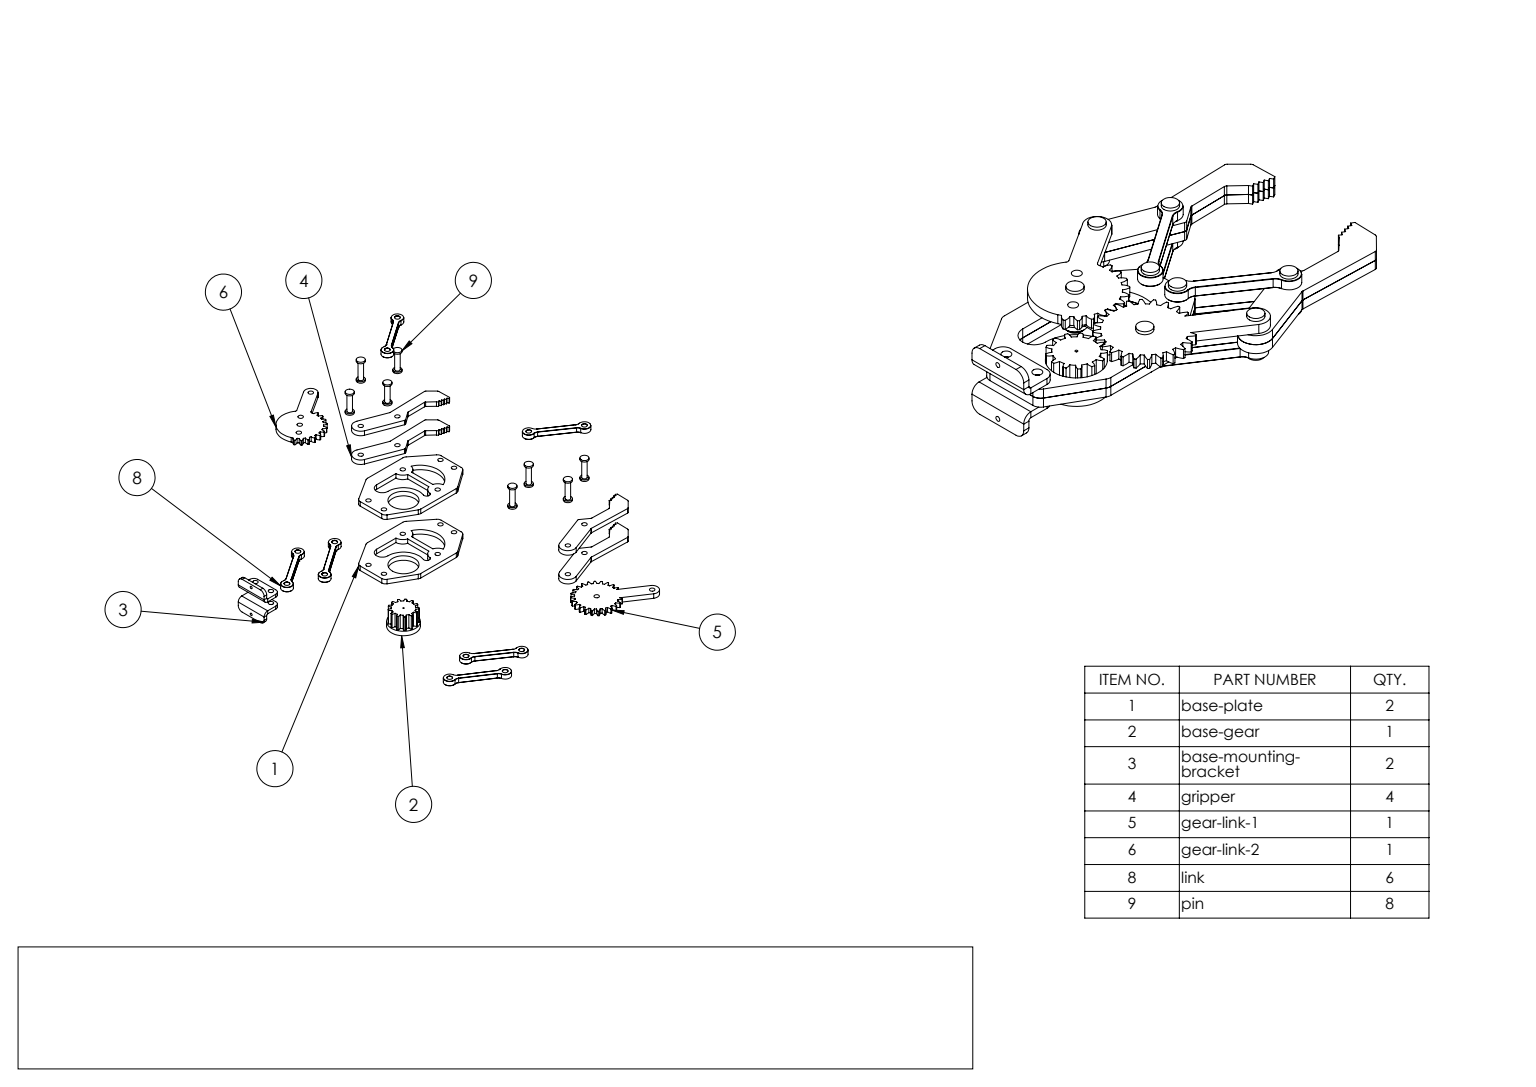
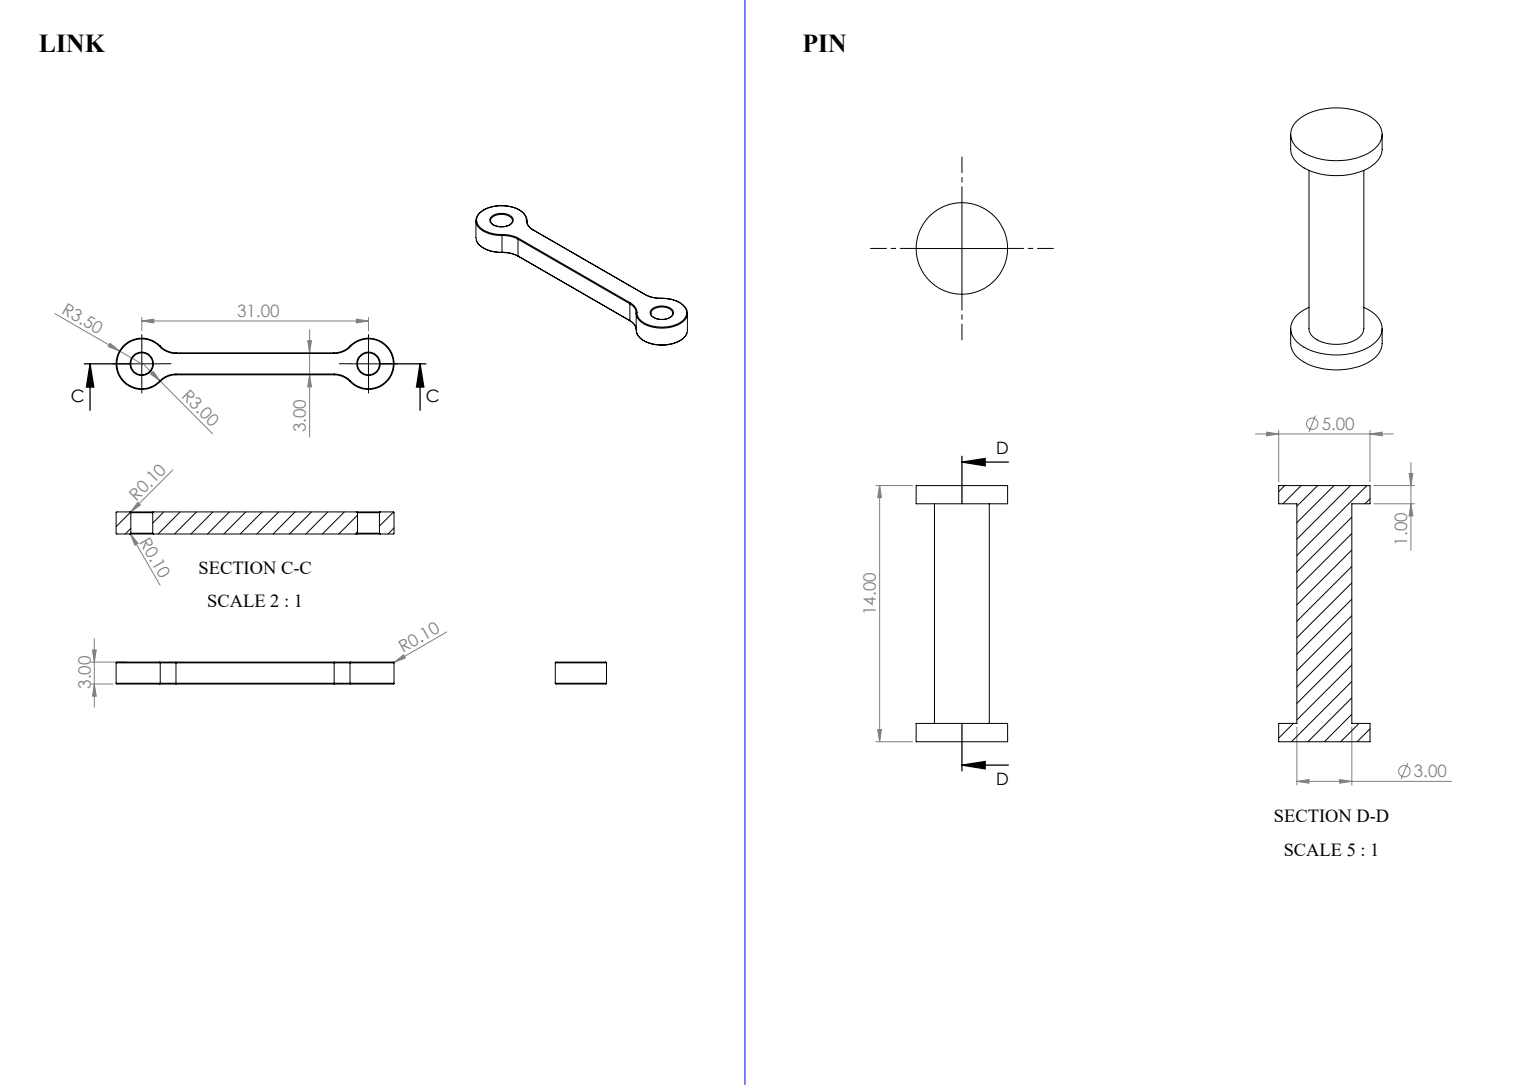
ISO-10303-21;
HEADER;
FILE_DESCRIPTION (('STEP AP214'),
    '1' );
FILE_NAME ('MAT-047',
    '2026-10-11T23:18:24',
    ( '' ),
    ( '' ),
    'SwSTEP 2.0',
    'SolidWorks 2021',
    '' );
FILE_SCHEMA (( 'AUTOMOTIVE_DESIGN' ));
ENDSEC;

DATA;
#1 = DIRECTION ( 'NONE',  ( 0.000000000000000000, 0.000000000000000000, -1.000000000000000000 ) ) ;
#2 = DIRECTION ( 'NONE',  ( 0.000000000000000000, 1.000000000000000000, 0.000000000000000000 ) ) ;
#3 = ORIENTED_EDGE ( 'NONE', *, *, #624, .T. ) ;
#4 = ORIENTED_EDGE ( 'NONE', *, *, #10369, .T. ) ;
#5 = FACE_OUTER_BOUND ( 'NONE', #2599, .T. ) ;
#6 = CIRCLE ( 'NONE', #7892, 1.600000000000000311 ) ;
#7 = EDGE_CURVE ( 'NONE', #479, #8134, #9794, .T. ) ;
#8 = ORIENTED_EDGE ( 'NONE', *, *, #949, .F. ) ;
#9 = FACE_BOUND ( 'NONE', #6807, .T. ) ;
#10 = B_SPLINE_CURVE_WITH_KNOTS ( 'NONE', 3,
 ( #6640, #5405, #12919, #3466 ),
 .UNSPECIFIED., .F., .F.,
 ( 4, 4 ),
 ( 0.1547128134717859205, 1.000000000000000000 ),
 .UNSPECIFIED. ) ;
#11 = PLANE ( 'NONE',  #4028 ) ;
#12 = DIRECTION ( 'NONE',  ( 0.000000000000000000, 0.000000000000000000, 1.000000000000000000 ) ) ;
#13 = CARTESIAN_POINT ( 'NONE',  ( 0.000000000000000000, 3.000000000000000000, 0.000000000000000000 ) ) ;
#14 = AXIS2_PLACEMENT_3D ( 'NONE', #3049, #7055, #9450 ) ;
#15 = CARTESIAN_POINT ( 'NONE',  ( 45.22938609343211880, 3.000000000000000000, -15.43472716196784233 ) ) ;
#16 = AXIS2_PLACEMENT_3D ( 'NONE', #3877, #7054, #1824 ) ;
#17 = CARTESIAN_POINT ( 'NONE',  ( 2.525608486058770641, 0.09999999999999982514, -2.423076923076923350 ) ) ;
#18 = EDGE_LOOP ( 'NONE', ( #222, #3036 ) ) ;
#19 = DIRECTION ( 'NONE',  ( -0.000000000000000000, -1.000000000000000000, -0.000000000000000000 ) ) ;
#20 = VERTEX_POINT ( 'NONE', #10251 ) ;
#21 = B_SPLINE_CURVE_WITH_KNOTS ( 'NONE', 3,
 ( #12632, #11655, #3183, #102 ),
 .UNSPECIFIED., .F., .F.,
 ( 4, 4 ),
 ( 0.1547128134717859205, 1.000000000000000000 ),
 .UNSPECIFIED. ) ;
#22 = ORIENTED_EDGE ( 'NONE', *, *, #1316, .F. ) ;
#23 = FACE_OUTER_BOUND ( 'NONE', #9551, .T. ) ;
#24 = EDGE_CURVE ( 'NONE', #4332, #3918, #6675, .T. ) ;
#25 = ORIENTED_EDGE ( 'NONE', *, *, #7176, .T. ) ;
#26 = AXIS2_PLACEMENT_3D ( 'NONE', #4384, #4937, #13276 ) ;
#27 = AXIS2_PLACEMENT_3D ( 'NONE', #4341, #12886, #6396 ) ;
#28 = DIRECTION ( 'NONE',  ( 0.000000000000000000, 1.000000000000000000, 0.000000000000000000 ) ) ;
#29 = ADVANCED_FACE ( 'NONE', ( #6308 ), #10384, .T. ) ;
#30 = DIRECTION ( 'NONE',  ( -0.000000000000000000, -1.000000000000000000, -0.000000000000000000 ) ) ;
#31 = EDGE_CURVE ( 'NONE', #5801, #5272, #8241, .T. ) ;
#32 = CARTESIAN_POINT ( 'NONE',  ( 2.458659560121117416, 9.000000000000000000, -8.136645080586040635 ) ) ;
#33 = LINE ( 'NONE', #12635, #7280 ) ;
#34 = CARTESIAN_POINT ( 'NONE',  ( 6.660877044263387781, 3.000000000000000000, -11.16999893002129696 ) ) ;
#35 = DIRECTION ( 'NONE',  ( 0.000000000000000000, 1.000000000000000000, 0.000000000000000000 ) ) ;
#36 = CARTESIAN_POINT ( 'NONE',  ( -3.835481108877868195, 0.000000000000000000, 5.554420281491219136 ) ) ;
#37 = FACE_OUTER_BOUND ( 'NONE', #7927, .T. ) ;
#38 = ORIENTED_EDGE ( 'NONE', *, *, #5654, .F. ) ;
#39 = CYLINDRICAL_SURFACE ( 'NONE', #3345, 6.750000000000000888 ) ;
#40 = AXIS2_PLACEMENT_3D ( 'NONE', #1430, #2390, #10728 ) ;
#41 = VECTOR ( 'NONE', #1784, 1000.000000000000000 ) ;
#42 = EDGE_LOOP ( 'NONE', ( #11575, #10640, #9047, #10732 ) ) ;
#43 = VERTEX_POINT ( 'NONE', #6242 ) ;
#44 = EDGE_CURVE ( 'NONE', #672, #1296, #10164, .T. ) ;
#45 = VERTEX_POINT ( 'NONE', #5075 ) ;
#46 = EDGE_LOOP ( 'NONE', ( #628, #4486, #10003, #7666 ) ) ;
#47 = FACE_BOUND ( 'NONE', #7549, .T. ) ;
#48 = DIRECTION ( 'NONE',  ( 0.000000000000000000, 1.000000000000000000, 0.000000000000000000 ) ) ;
#49 = EDGE_CURVE ( 'NONE', #1339, #3948, #9205, .T. ) ;
#50 = CIRCLE ( 'NONE', #7727, 3.000000000000000000 ) ;
#51 = FACE_OUTER_BOUND ( 'NONE', #63, .T. ) ;
#52 = B_SPLINE_CURVE_WITH_KNOTS ( 'NONE', 3,
 ( #4525, #5550, #8714, #7882 ),
 .UNSPECIFIED., .F., .F.,
 ( 4, 4 ),
 ( 0.6363612417694253232, 0.6657793188270956231 ),
 .UNSPECIFIED. ) ;
#53 = CARTESIAN_POINT ( 'NONE',  ( 0.000000000000000000, 3.000000000000000000, 0.000000000000000000 ) ) ;
#54 = CARTESIAN_POINT ( 'NONE',  ( 41.29994854050690378, 3.000000000000000000, -5.141175130212632283 ) ) ;
#55 = CARTESIAN_POINT ( 'NONE',  ( -4.564691384634503635, 3.000000000000000000, 12.76342233970727769 ) ) ;
#56 = EDGE_LOOP ( 'NONE', ( #12824, #10379, #9147, #863 ) ) ;
#57 = ORIENTED_EDGE ( 'NONE', *, *, #11037, .F. ) ;
#58 = VECTOR ( 'NONE', #8688, 1000.000000000000000 ) ;
#59 = ADVANCED_FACE ( 'NONE', ( #12400 ), #9143, .T. ) ;
#60 = DIRECTION ( 'NONE',  ( -0.000000000000000000, -1.000000000000000000, -0.000000000000000000 ) ) ;
#61 = EDGE_CURVE ( 'NONE', #8421, #357, #9412, .T. ) ;
#62 = B_SPLINE_SURFACE_WITH_KNOTS ( 'NONE', 3, 1, ( 
 ( #3640, #12274 ),
 ( #3773, #7979 ),
 ( #12201, #7023 ),
 ( #11219, #1791 ) ),
 .UNSPECIFIED., .F., .F., .F.,
 ( 4, 4 ),
 ( 2, 2 ),
 ( 0.1276832474596304168, 1.000000000000000000 ),
 ( 0.000000000000000000, 1.000000000000000000 ),
 .UNSPECIFIED. ) ;
#63 = EDGE_LOOP ( 'NONE', ( #5168, #8136, #3931, #2663 ) ) ;
#64 = DIRECTION ( 'NONE',  ( 0.000000000000000000, 1.000000000000000000, 0.000000000000000000 ) ) ;
#65 = DIRECTION ( 'NONE',  ( 0.000000000000000000, 0.000000000000000000, 1.000000000000000000 ) ) ;
#66 = AXIS2_PLACEMENT_3D ( 'NONE', #5412, #190, #2837 ) ;
#67 = ITEM_DEFINED_TRANSFORMATION ( 'NONE', 'NONE', #10472,  #10007 ) ;
#68 = VECTOR ( 'NONE', #1053, 1000.000000000000000 ) ;
#69 = AXIS2_PLACEMENT_3D ( 'NONE', #2315, #6513, #10716 ) ;
#70 = DIRECTION ( 'NONE',  ( 0.000000000000000000, -1.000000000000000000, 0.000000000000000000 ) ) ;
#71 = CARTESIAN_POINT ( 'NONE',  ( 2.161962830978782613, 0.000000000000000000, 14.08504230442586369 ) ) ;
#72 = CARTESIAN_POINT ( 'NONE',  ( 10.00000000000000000, 2.749999999999999112, -10.00000000000000178 ) ) ;
#73 = LINE ( 'NONE', #7490, #793 ) ;
#74 = CARTESIAN_POINT ( 'NONE',  ( 5.170206418547656391, 3.000000000000000000, 13.27898586450067064 ) ) ;
#75 = VERTEX_POINT ( 'NONE', #8304 ) ;
#76 = VERTEX_POINT ( 'NONE', #2943 ) ;
#77 = ORIENTED_EDGE ( 'NONE', *, *, #13230, .T. ) ;
#78 = FACE_OUTER_BOUND ( 'NONE', #11147, .T. ) ;
#79 = AXIS2_PLACEMENT_3D ( 'NONE', #10784, #8462, #2387 ) ;
#80 = AXIS2_PLACEMENT_3D ( 'NONE', #518, #2715, #10017 ) ;
#81 = EDGE_LOOP ( 'NONE', ( #694, #11176, #5108, #897 ) ) ;
#82 = B_SPLINE_SURFACE_WITH_KNOTS ( 'NONE', 2, 1, ( 
 ( #10714, #1415 ),
 ( #319, #8701 ),
 ( #12978, #11750 ) ),
 .UNSPECIFIED., .F., .F., .F.,
 ( 3, 3 ),
 ( 2, 2 ),
 ( 0.000000000000000000, 1.000000000000000000 ),
 ( 0.000000000000000000, 1.000000000000000000 ),
 .UNSPECIFIED. ) ;
#83 = LINE ( 'NONE', #6330, #6796 ) ;
#84 =( NAMED_UNIT ( * ) SI_UNIT ( $, .STERADIAN. ) SOLID_ANGLE_UNIT ( ) );
#85 = DIRECTION ( 'NONE',  ( 0.7772490812545796990, 0.000000000000000000, 0.6291930273683203900 ) ) ;
#86 = CIRCLE ( 'NONE', #7751, 1.600000000000000311 ) ;
#87 = CARTESIAN_POINT ( 'NONE',  ( -3.835481108877868195, 9.000000000000000000, 5.554420281491219136 ) ) ;
#88 = PRODUCT_DEFINITION_SHAPE ( 'NONE', 'NONE',  #13602 ) ;
#89 = CIRCLE ( 'NONE', #4911, 1.500000000000000222 ) ;
#90 = CARTESIAN_POINT ( 'NONE',  ( 13.04554897075799502, 0.000000000000000000, 5.733772933379473358 ) ) ;
#91 = LINE ( 'NONE', #6076, #1434 ) ;
#92 = EDGE_CURVE ( 'NONE', #5359, #2558, #6205, .T. ) ;
#93 = CIRCLE ( 'NONE', #9082, 12.08999999999737085 ) ;
#94 = ORIENTED_EDGE ( 'NONE', *, *, #1256, .F. ) ;
#95 = FILL_AREA_STYLE_COLOUR ( '', #505 ) ;
#96 = ORIENTED_EDGE ( 'NONE', *, *, #10741, .F. ) ;
#97 = VERTEX_POINT ( 'NONE', #7219 ) ;
#98 = ORIENTED_EDGE ( 'NONE', *, *, #5069, .T. ) ;
#99 = CARTESIAN_POINT ( 'NONE',  ( 0.000000000000000000, 0.000000000000000000, 0.000000000000000000 ) ) ;
#100 = ORIENTED_EDGE ( 'NONE', *, *, #3165, .F. ) ;
#101 = VECTOR ( 'NONE', #278, 1000.000000000000000 ) ;
#102 = CARTESIAN_POINT ( 'NONE',  ( -14.08504230442587790, 0.000000000000000000, -2.161962830978695571 ) ) ;
#103 =( LENGTH_UNIT ( ) NAMED_UNIT ( * ) SI_UNIT ( .MILLI., .METRE. ) );
#104 = DIRECTION ( 'NONE',  ( -0.000000000000000000, -1.000000000000000000, -0.000000000000000000 ) ) ;
#105 = CARTESIAN_POINT ( 'NONE',  ( 17.00000000000000711, 0.000000000000000000, 12.57924256039205524 ) ) ;
#106 = CARTESIAN_POINT ( 'NONE',  ( 12.89546620003432764, 3.000000000000000000, -4.733530556166651415 ) ) ;
#107 = DIRECTION ( 'NONE',  ( -0.000000000000000000, -1.000000000000000000, -0.000000000000000000 ) ) ;
#108 = EDGE_CURVE ( 'NONE', #3124, #12047, #7960, .T. ) ;
#109 = CYLINDRICAL_SURFACE ( 'NONE', #708, 12.08999999999737440 ) ;
#110 = CARTESIAN_POINT ( 'NONE',  ( -8.430890348300632553, 0.000000000000000000, -11.48836750521723538 ) ) ;
#111 = ADVANCED_FACE ( 'NONE', ( #10454 ), #11355, .F. ) ;
#112 = EDGE_LOOP ( 'NONE', ( #12398, #1817, #7232, #6779 ) ) ;
#113 = EDGE_CURVE ( 'NONE', #9400, #10019, #10289, .T. ) ;
#114 = PLANE ( 'NONE',  #5341 ) ;
#115 = AXIS2_PLACEMENT_3D ( 'NONE', #683, #10945, #4876 ) ;
#116 = VERTEX_POINT ( 'NONE', #11558 ) ;
#117 = VERTEX_POINT ( 'NONE', #1849 ) ;
#118 = ADVANCED_FACE ( 'NONE', ( #1922 ), #5010, .T. ) ;
#119 = EDGE_LOOP ( 'NONE', ( #1078, #10235 ) ) ;
#120 = CARTESIAN_POINT ( 'NONE',  ( 6.000000000000008882, 3.000000000000000000, 28.50000000000000000 ) ) ;
#121 = VECTOR ( 'NONE', #10076, 1000.000000000000000 ) ;
#122 = AXIS2_PLACEMENT_3D ( 'NONE', #7328, #11458, #1060 ) ;
#123 =( NAMED_UNIT ( * ) SI_UNIT ( $, .STERADIAN. ) SOLID_ANGLE_UNIT ( ) );
#124 = CARTESIAN_POINT ( 'NONE',  ( -20.74285254778206422, 3.000000000000000000, 14.10762559394868454 ) ) ;
#125 = EDGE_CURVE ( 'NONE', #3742, #5918, #6114, .T. ) ;
#126 = CARTESIAN_POINT ( 'NONE',  ( 7.659717769608228366, -1.694065894508600678E-18, -2.099897208369672530 ) ) ;
#127 = CARTESIAN_POINT ( 'NONE',  ( -13.73660796332618261, 3.000000000000000000, -6.025412986832017204 ) ) ;
#128 = LINE ( 'NONE', #8180, #4659 ) ;
#129 = ORIENTED_EDGE ( 'NONE', *, *, #3513, .F. ) ;
#130 = EDGE_CURVE ( 'NONE', #748, #10888, #9495, .T. ) ;
#131 = AXIS2_PLACEMENT_3D ( 'NONE', #780, #12143, #5869 ) ;
#132 = ORIENTED_EDGE ( 'NONE', *, *, #11466, .T. ) ;
#133 = ADVANCED_FACE ( 'NONE', ( #11682 ), #12860, .T. ) ;
#134 = DIRECTION ( 'NONE',  ( 0.000000000000000000, 0.000000000000000000, 1.000000000000000000 ) ) ;
#135 = ORIENTED_EDGE ( 'NONE', *, *, #11819, .F. ) ;
#136 = CYLINDRICAL_SURFACE ( 'NONE', #4471, 8.499999999999996447 ) ;
#137 = DIRECTION ( 'NONE',  ( 0.000000000000000000, 0.000000000000000000, -1.000000000000000000 ) ) ;
#138 = AXIS2_PLACEMENT_3D ( 'NONE', #9774, #352, #10185 ) ;
#139 = DIRECTION ( 'NONE',  ( -0.000000000000000000, -1.000000000000000000, -0.000000000000000000 ) ) ;
#140 = CARTESIAN_POINT ( 'NONE',  ( 12.03251085770905959, 3.000000000000000000, 3.999999998926332179 ) ) ;
#141 = EDGE_CURVE ( 'NONE', #20, #6815, #252, .T. ) ;
#142 = FACE_OUTER_BOUND ( 'NONE', #3099, .T. ) ;
#143 = DIRECTION ( 'NONE',  ( -0.6291930273683257191, 0.000000000000000000, 0.7772490812545752581 ) ) ;
#144 = VERTEX_POINT ( 'NONE', #5273 ) ;
#145 = ORIENTED_EDGE ( 'NONE', *, *, #11996, .T. ) ;
#146 = CARTESIAN_POINT ( 'NONE',  ( 12.03251085770905959, 0.000000000000000000, 3.999999998926332179 ) ) ;
#147 = EDGE_LOOP ( 'NONE', ( #10873, #12283, #1803, #7065 ) ) ;
#148 = DIRECTION ( 'NONE',  ( 0.000000000000000000, 1.000000000000000000, 0.000000000000000000 ) ) ;
#149 = ORIENTED_EDGE ( 'NONE', *, *, #3145, .T. ) ;
#150 = FACE_BOUND ( 'NONE', #4431, .T. ) ;
#151 = EDGE_CURVE ( 'NONE', #10361, #2347, #9475, .T. ) ;
#152 = CARTESIAN_POINT ( 'NONE',  ( 4.564691384634508964, 3.000000000000000000, -12.76342233970727413 ) ) ;
#153 = ADVANCED_FACE ( 'NONE', ( #4377 ), #6607, .F. ) ;
#154 = PLANE ( 'NONE',  #12644 ) ;
#155 = CARTESIAN_POINT ( 'NONE',  ( -7.155006492985575228, 0.000000000000000000, -1.740452503570284915 ) ) ;
#156 = CARTESIAN_POINT ( 'NONE',  ( 0.5501230721522984979, 3.000000000000000000, -12.98835496148321766 ) ) ;
#157 = CARTESIAN_POINT ( 'NONE',  ( -9.573149624528719315, 0.000000000000000000, -8.795158114916407754 ) ) ;
#158 = ORIENTED_EDGE ( 'NONE', *, *, #6115, .F. ) ;
#159 = CARTESIAN_POINT ( 'NONE',  ( -1.557181465540760534, 3.000000000000000000, -14.16466328168009703 ) ) ;
#160 = ORIENTED_EDGE ( 'NONE', *, *, #10207, .F. ) ;
#161 = ORIENTED_EDGE ( 'NONE', *, *, #7234, .F. ) ;
#162 = B_SPLINE_SURFACE_WITH_KNOTS ( 'NONE', 3, 1, ( 
 ( #10319, #7359 ),
 ( #1025, #5084 ),
 ( #8312, #12538 ),
 ( #2123, #4325 ) ),
 .UNSPECIFIED., .F., .F., .F.,
 ( 4, 4 ),
 ( 2, 2 ),
 ( 0.000000000000000000, 0.5855695330273008592 ),
 ( 0.000000000000000000, 1.000000000000000000 ),
 .UNSPECIFIED. ) ;
#163 = ORIENTED_EDGE ( 'NONE', *, *, #6136, .T. ) ;
#164 = DIRECTION ( 'NONE',  ( 0.000000000000000000, 0.000000000000000000, 1.000000000000000000 ) ) ;
#165 = B_SPLINE_CURVE_WITH_KNOTS ( 'NONE', 3,
 ( #7734, #1615, #8698, #11948 ),
 .UNSPECIFIED., .F., .F.,
 ( 4, 4 ),
 ( 0.000000000000000000, 0.5855695330273008592 ),
 .UNSPECIFIED. ) ;
#166 = ORIENTED_EDGE ( 'NONE', *, *, #10741, .T. ) ;
#167 = DIRECTION ( 'NONE',  ( -1.261435711112880913E-16, -0.000000000000000000, -1.000000000000000000 ) ) ;
#168 = DIRECTION ( 'NONE',  ( -0.000000000000000000, -1.000000000000000000, -0.000000000000000000 ) ) ;
#169 = CARTESIAN_POINT ( 'NONE',  ( 2.604399508763944660, 3.000000000000000000, -11.80615107470197600 ) ) ;
#170 = DIRECTION ( 'NONE',  ( -2.602085213965199795E-16, 2.891205793294684736E-16, -1.000000000000000000 ) ) ;
#171 = B_SPLINE_CURVE_WITH_KNOTS ( 'NONE', 3,
 ( #9035, #3811, #13254, #8012 ),
 .UNSPECIFIED., .F., .F.,
 ( 4, 4 ),
 ( 0.09090310649439187207, 0.1203211835519651524 ),
 .UNSPECIFIED. ) ;
#172 = CARTESIAN_POINT ( 'NONE',  ( 12.46219022525837694, 3.000000000000000000, -4.344528055836598845 ) ) ;
#173 = CARTESIAN_POINT ( 'NONE',  ( -8.795158114916672432, 3.000000000000000000, -9.573149624528774382 ) ) ;
#174 = CYLINDRICAL_SURFACE ( 'NONE', #2308, 12.08999999999737440 ) ;
#175 = VERTEX_POINT ( 'NONE', #12924 ) ;
#176 = CARTESIAN_POINT ( 'NONE',  ( 7.500000000000003553, 0.000000000000000000, 1.399999999999998579 ) ) ;
#177 = B_SPLINE_SURFACE_WITH_KNOTS ( 'NONE', 3, 1, ( 
 ( #3234, #4074 ),
 ( #11315, #11514 ),
 ( #3171, #9382 ),
 ( #841, #13580 ) ),
 .UNSPECIFIED., .F., .F., .F.,
 ( 4, 4 ),
 ( 2, 2 ),
 ( 0.1547128134717859205, 1.000000000000000000 ),
 ( 0.000000000000000000, 1.000000000000000000 ),
 .UNSPECIFIED. ) ;
#178 = ORIENTED_EDGE ( 'NONE', *, *, #12277, .T. ) ;
#179 = ORIENTED_EDGE ( 'NONE', *, *, #10718, .F. ) ;
#180 = VERTEX_POINT ( 'NONE', #12788 ) ;
#181 = EDGE_CURVE ( 'NONE', #11338, #1291, #2903, .T. ) ;
#182 = CARTESIAN_POINT ( 'NONE',  ( 7.151505841916629080, 9.000000000000000000, 1.752496229622501511 ) ) ;
#183 = CARTESIAN_POINT ( 'NONE',  ( 2.458659560121116527, 0.000000000000000000, -8.136645080586040635 ) ) ;
#184 = CARTESIAN_POINT ( 'NONE',  ( -7.144272221052618832, 9.000000000000000000, 1.784003156764502940 ) ) ;
#185 = CARTESIAN_POINT ( 'NONE',  ( 1.557181465540672161, 3.000000000000000000, -14.16466328168010591 ) ) ;
#186 = DIRECTION ( 'NONE',  ( 0.000000000000000000, 1.000000000000000000, 0.000000000000000000 ) ) ;
#187 = CARTESIAN_POINT ( 'NONE',  ( 4.355042381134426321, 9.000000000000000000, 7.299562031966228659 ) ) ;
#188 = ORIENTED_EDGE ( 'NONE', *, *, #12912, .F. ) ;
#189 = ORIENTED_EDGE ( 'NONE', *, *, #8491, .T. ) ;
#190 = DIRECTION ( 'NONE',  ( -0.000000000000000000, -1.000000000000000000, -0.000000000000000000 ) ) ;
#191 = ADVANCED_FACE ( 'NONE', ( #1279 ), #11366, .T. ) ;
#192 = EDGE_CURVE ( 'NONE', #3774, #5500, #7308, .T. ) ;
#193 = ORIENTED_EDGE ( 'NONE', *, *, #5488, .T. ) ;
#194 = CARTESIAN_POINT ( 'NONE',  ( -8.158651161643904359, 3.000000000000000000, -8.922136023539605887 ) ) ;
#195 = PRODUCT_DEFINITION_SHAPE ( 'NONE', 'NONE',  #13619 ) ;
#196 = CARTESIAN_POINT ( 'NONE',  ( 13.40069634612381044, 0.000000000000000000, 2.546644602219900300 ) ) ;
#197 = EDGE_CURVE ( 'NONE', #3277, #3201, #3548, .T. ) ;
#198 = EDGE_CURVE ( 'NONE', #9031, #937, #1143, .T. ) ;
#199 = DIRECTION ( 'NONE',  ( -0.000000000000000000, -1.000000000000000000, -0.000000000000000000 ) ) ;
#200 = CARTESIAN_POINT ( 'NONE',  ( 0.000000000000000000, 0.000000000000000000, 0.000000000000000000 ) ) ;
#201 = DIRECTION ( 'NONE',  ( 0.6291930273683254971, 0.000000000000000000, -0.7772490812545754801 ) ) ;
#202 = CARTESIAN_POINT ( 'NONE',  ( 0.000000000000000000, 0.09999999999999982514, 0.000000000000000000 ) ) ;
#203 = DIRECTION ( 'NONE',  ( 0.000000000000000000, 0.000000000000000000, 1.000000000000000000 ) ) ;
#204 = ORIENTED_EDGE ( 'NONE', *, *, #9463, .T. ) ;
#205 = VERTEX_POINT ( 'NONE', #6448 ) ;
#206 = ORIENTED_EDGE ( 'NONE', *, *, #10658, .F. ) ;
#207 = CARTESIAN_POINT ( 'NONE',  ( 12.08646469655232636, 3.000000000000000000, -8.883544964652022813 ) ) ;
#208 = EDGE_CURVE ( 'NONE', #1513, #12626, #879, .T. ) ;
#209 = ORIENTED_EDGE ( 'NONE', *, *, #7248, .F. ) ;
#210 = EDGE_CURVE ( 'NONE', #8040, #5490, #481, .T. ) ;
#211 = DIRECTION ( 'NONE',  ( 0.000000000000000000, 0.000000000000000000, -1.000000000000000000 ) ) ;
#212 = EDGE_CURVE ( 'NONE', #8880, #8783, #12663, .T. ) ;
#213 = DIRECTION ( 'NONE',  ( 0.000000000000000000, 1.000000000000000000, 0.000000000000000000 ) ) ;
#214 = LINE ( 'NONE', #2474, #9546 ) ;
#215 = CARTESIAN_POINT ( 'NONE',  ( -2.264806262022998062, 0.000000000000000000, -14.82803603298499340 ) ) ;
#216 = CARTESIAN_POINT ( 'NONE',  ( -13.33579367773357482, 0.000000000000000000, 2.428572470324200427 ) ) ;
#217 = FACE_OUTER_BOUND ( 'NONE', #13506, .T. ) ;
#218 = ORIENTED_EDGE ( 'NONE', *, *, #842, .T. ) ;
#219 = ORIENTED_EDGE ( 'NONE', *, *, #9373, .F. ) ;
#220 = EDGE_LOOP ( 'NONE', ( #4199, #4816, #462, #4259 ) ) ;
#221 = VECTOR ( 'NONE', #9431, 1000.000000000000000 ) ;
#222 = ORIENTED_EDGE ( 'NONE', *, *, #10239, .T. ) ;
#223 = DIRECTION ( 'NONE',  ( -0.000000000000000000, -1.000000000000000000, -0.000000000000000000 ) ) ;
#224 = EDGE_CURVE ( 'NONE', #1339, #3538, #12385, .T. ) ;
#225 = ORIENTED_EDGE ( 'NONE', *, *, #4550, .T. ) ;
#226 = FACE_OUTER_BOUND ( 'NONE', #1132, .T. ) ;
#227 = DIRECTION ( 'NONE',  ( 0.000000000000000000, 0.000000000000000000, -1.000000000000000000 ) ) ;
#228 = CARTESIAN_POINT ( 'NONE',  ( -13.52637830886122572, 3.000000000000000000, -2.928250210355275218 ) ) ;
#229 = DIRECTION ( 'NONE',  ( 1.000000000000000000, 0.000000000000000000, 1.224646799147353207E-16 ) ) ;
#230 = AXIS2_PLACEMENT_3D ( 'NONE', #6911, #11119, #1688 ) ;
#231 = DIRECTION ( 'NONE',  ( -0.000000000000000000, -1.000000000000000000, -0.000000000000000000 ) ) ;
#232 = CARTESIAN_POINT ( 'NONE',  ( 2.928250210355320959, 3.000000000000000000, -13.52637830886121506 ) ) ;
#233 = CARTESIAN_POINT ( 'NONE',  ( 9.600126836553261711, 3.000000000000000000, 8.482622935103766082 ) ) ;
#234 = CARTESIAN_POINT ( 'NONE',  ( -20.74285254778206422, 3.000000000000000000, 14.10762559394868454 ) ) ;
#235 = ORIENTED_EDGE ( 'NONE', *, *, #9698, .T. ) ;
#236 = CARTESIAN_POINT ( 'NONE',  ( 6.970598036433451661, 3.000000000000000000, -10.97318381393796294 ) ) ;
#237 = ORIENTED_EDGE ( 'NONE', *, *, #7398, .T. ) ;
#238 = ORIENTED_EDGE ( 'NONE', *, *, #208, .T. ) ;
#239 = AXIS2_PLACEMENT_3D ( 'NONE', #13533, #6287, #2844 ) ;
#240 = ORIENTED_EDGE ( 'NONE', *, *, #11722, .F. ) ;
#241 = DIRECTION ( 'NONE',  ( 0.000000000000000000, 1.000000000000000000, -0.000000000000000000 ) ) ;
#242 = SURFACE_STYLE_FILL_AREA ( #6365 ) ;
#243 = CARTESIAN_POINT ( 'NONE',  ( 7.500000000000003553, 3.000000000000000000, 13.39999999999999858 ) ) ;
#244 = VECTOR ( 'NONE', #1493, 1000.000000000000000 ) ;
#245 = LINE ( 'NONE', #7737, #3762 ) ;
#246 = CARTESIAN_POINT ( 'NONE',  ( 7.723663868796767140, 0.000000000000000000, 11.13895890373327191 ) ) ;
#247 = CIRCLE ( 'NONE', #1345, 13.50000000000000178 ) ;
#248 = CARTESIAN_POINT ( 'NONE',  ( 0.4639228963249704130, 0.000000000000000000, 8.487330295579726069 ) ) ;
#249 = ORIENTED_EDGE ( 'NONE', *, *, #2547, .F. ) ;
#250 = ADVANCED_FACE ( 'NONE', ( #4318 ), #7479, .T. ) ;
#251 = ORIENTED_EDGE ( 'NONE', *, *, #1134, .T. ) ;
#252 = LINE ( 'NONE', #10721, #2679 ) ;
#253 = AXIS2_PLACEMENT_3D ( 'NONE', #1336, #11952, #4576 ) ;
#254 = AXIS2_PLACEMENT_3D ( 'NONE', #5963, #13478, #3894 ) ;
#255 = ORIENTED_EDGE ( 'NONE', *, *, #3006, .T. ) ;
#256 = DIRECTION ( 'NONE',  ( -0.000000000000000000, -1.000000000000000000, -0.000000000000000000 ) ) ;
#257 = LINE ( 'NONE', #1752, #8132 ) ;
#258 = CARTESIAN_POINT ( 'NONE',  ( 5.985774866078160450, 9.000000000000000000, 3.119775513178307147 ) ) ;
#259 = CARTESIAN_POINT ( 'NONE',  ( -6.970598036433426792, 3.000000000000000000, -10.97318381393771780 ) ) ;
#260 = DIRECTION ( 'NONE',  ( 0.000000000000000000, 1.000000000000000000, 0.000000000000000000 ) ) ;
#261 = CIRCLE ( 'NONE', #2893, 12.08999999999737440 ) ;
#262 = B_SPLINE_SURFACE_WITH_KNOTS ( 'NONE', 3, 1, ( 
 ( #1876, #12212 ),
 ( #3923, #7034 ),
 ( #7178, #4068 ),
 ( #11374, #6196 ) ),
 .UNSPECIFIED., .F., .F., .F.,
 ( 4, 4 ),
 ( 2, 2 ),
 ( 0.1276832474596238665, 1.000000000000000000 ),
 ( 0.000000000000000000, 1.000000000000000000 ),
 .UNSPECIFIED. ) ;
#263 = FACE_OUTER_BOUND ( 'NONE', #2351, .T. ) ;
#264 = EDGE_CURVE ( 'NONE', #8710, #692, #9279, .T. ) ;
#265 = CARTESIAN_POINT ( 'NONE',  ( -7.798201703419555209, 3.000000000000000000, -30.99999999999999289 ) ) ;
#266 = EDGE_LOOP ( 'NONE', ( #10134, #2477, #2333, #5399 ) ) ;
#267 = ORIENTED_EDGE ( 'NONE', *, *, #5862, .F. ) ;
#268 = EDGE_LOOP ( 'NONE', ( #11853, #9948, #1249, #11697 ) ) ;
#269 = ORIENTED_EDGE ( 'NONE', *, *, #8193, .F. ) ;
#270 = CARTESIAN_POINT ( 'NONE',  ( 0.5400000000008001733, 0.000000000000000000, 12.07793442604883616 ) ) ;
#271 = EDGE_CURVE ( 'NONE', #7435, #2693, #13455, .T. ) ;
#272 = EDGE_LOOP ( 'NONE', ( #9491, #3874, #11052, #3338, #8276, #2839, #644, #11022, #10546, #6323, #4126, #5305, #5722, #5484, #10567, #12738, #3922, #6142, #1219, #3241, #11942, #4726, #6997, #1679, #13263, #12542, #5199, #9334, #7477, #1094, #5617, #8851, #4788, #11957, #10551, #9765, #5855, #13484, #4229, #12910, #8520, #970, #6174, #5838, #218, #6140, #7889, #11447, #8596, #13140, #12291, #13402, #12003, #12804 ) ) ;
#273 = LINE ( 'NONE', #11625, #11249 ) ;
#274 = CIRCLE ( 'NONE', #4001, 1.500000000000000222 ) ;
#275 = CARTESIAN_POINT ( 'NONE',  ( 0.000000000000000000, 3.000000000000000000, 3.400000000000001243 ) ) ;
#276 = B_SPLINE_SURFACE_WITH_KNOTS ( 'NONE', 3, 1, ( 
 ( #10127, #2687 ),
 ( #3651, #10063 ),
 ( #632, #13233 ),
 ( #12213, #10958 ) ),
 .UNSPECIFIED., .F., .F., .F.,
 ( 4, 4 ),
 ( 2, 2 ),
 ( 0.000000000000000000, 0.5855695330273008592 ),
 ( 0.000000000000000000, 1.000000000000000000 ),
 .UNSPECIFIED. ) ;
#277 = CARTESIAN_POINT ( 'NONE',  ( 5.571313494980134173, 0.000000000000000000, -10.72979803820132005 ) ) ;
#278 = DIRECTION ( 'NONE',  ( -0.000000000000000000, -1.000000000000000000, -0.000000000000000000 ) ) ;
#279 = EDGE_CURVE ( 'NONE', #8354, #8278, #7045, .T. ) ;
#280 = CARTESIAN_POINT ( 'NONE',  ( -21.21140389626389577, 3.000000000000000000, -14.83930531255814955 ) ) ;
#281 = CARTESIAN_POINT ( 'NONE',  ( 5.452638258930520010, 3.000000000000000000, -13.97385902380752754 ) ) ;
#282 = ORIENTED_EDGE ( 'NONE', *, *, #5312, .T. ) ;
#283 = CIRCLE ( 'NONE', #2044, 3.399999999999999911 ) ;
#284 = VERTEX_POINT ( 'NONE', #2910 ) ;
#285 = AXIS2_PLACEMENT_3D ( 'NONE', #7655, #11797, #366 ) ;
#286 = VECTOR ( 'NONE', #8892, 1000.000000000000000 ) ;
#287 = ORIENTED_EDGE ( 'NONE', *, *, #2381, .F. ) ;
#288 = VERTEX_POINT ( 'NONE', #5039 ) ;
#289 = DIRECTION ( 'NONE',  ( 0.7772490812545727046, 0.000000000000000000, 0.6291930273683288277 ) ) ;
#290 = EDGE_CURVE ( 'NONE', #11016, #1998, #3872, .T. ) ;
#291 = VERTEX_POINT ( 'NONE', #13245 ) ;
#292 = ORIENTED_EDGE ( 'NONE', *, *, #12896, .T. ) ;
#293 = CARTESIAN_POINT ( 'NONE',  ( 0.000000000000000000, 3.000000000000000000, 1.600000000000000311 ) ) ;
#294 = CIRCLE ( 'NONE', #2053, 12.08999999999737263 ) ;
#295 = CIRCLE ( 'NONE', #8842, 5.000000000000000000 ) ;
#296 = AXIS2_PLACEMENT_3D ( 'NONE', #2142, #10485, #1885 ) ;
#297 = LINE ( 'NONE', #4418, #7104 ) ;
#298 = DIRECTION ( 'NONE',  ( -0.000000000000000000, -1.000000000000000000, -0.000000000000000000 ) ) ;
#299 = B_SPLINE_CURVE_WITH_KNOTS ( 'NONE', 3,
 ( #9811, #1338, #2514, #4372 ),
 .UNSPECIFIED., .F., .F.,
 ( 4, 4 ),
 ( 0.1547128134717859205, 1.000000000000000000 ),
 .UNSPECIFIED. ) ;
#300 = FACE_BOUND ( 'NONE', #2086, .T. ) ;
#301 = EDGE_CURVE ( 'NONE', #13005, #4332, #5938, .T. ) ;
#302 = CARTESIAN_POINT ( 'NONE',  ( 10.33484986938308481, 3.000000000000000000, -8.771102293099065861 ) ) ;
#303 = EDGE_CURVE ( 'NONE', #781, #13268, #10919, .T. ) ;
#304 = DIRECTION ( 'NONE',  ( 0.000000000000000000, 1.000000000000000000, 0.000000000000000000 ) ) ;
#305 = ORIENTED_EDGE ( 'NONE', *, *, #3885, .F. ) ;
#306 = B_SPLINE_CURVE_WITH_KNOTS ( 'NONE', 3,
 ( #11706, #6473, #8390, #12616 ),
 .UNSPECIFIED., .F., .F.,
 ( 4, 4 ),
 ( 0.000000000000000000, 0.5855695330273008592 ),
 .UNSPECIFIED. ) ;
#307 = CARTESIAN_POINT ( 'NONE',  ( -8.914835885878282795, 0.000000000000000000, -11.11702303352191556 ) ) ;
#308 = ORIENTED_EDGE ( 'NONE', *, *, #11057, .T. ) ;
#309 = CIRCLE ( 'NONE', #12190, 12.08999999999737263 ) ;
#310 = EDGE_LOOP ( 'NONE', ( #4705, #3628, #1202, #9996 ) ) ;
#311 = CIRCLE ( 'NONE', #11742, 3.000000000000000000 ) ;
#312 = AXIS2_PLACEMENT_3D ( 'NONE', #8923, #4738, #13201 ) ;
#313 = VERTEX_POINT ( 'NONE', #10072 ) ;
#314 = DIRECTION ( 'NONE',  ( -0.000000000000000000, -1.000000000000000000, -0.000000000000000000 ) ) ;
#315 = LINE ( 'NONE', #6769, #11331 ) ;
#316 = DIRECTION ( 'NONE',  ( 0.000000000000000000, 0.000000000000000000, 1.000000000000000000 ) ) ;
#317 = CARTESIAN_POINT ( 'NONE',  ( 1.650143266773734796, 0.000000000000000000, -14.90895795148410841 ) ) ;
#318 = VECTOR ( 'NONE', #11914, 1000.000000000000000 ) ;
#319 = CARTESIAN_POINT ( 'NONE',  ( 5.741477348071313713, 3.000000000000000000, -13.86115248177180703 ) ) ;
#320 = DIRECTION ( 'NONE',  ( 0.000000000000000000, 1.000000000000000000, 0.000000000000000000 ) ) ;
#321 = EDGE_CURVE ( 'NONE', #11737, #6548, #895, .T. ) ;
#322 = DIRECTION ( 'NONE',  ( -0.000000000000000000, -1.000000000000000000, -0.000000000000000000 ) ) ;
#323 = EDGE_LOOP ( 'NONE', ( #13175, #3374, #10326, #9587 ) ) ;
#324 = ORIENTED_EDGE ( 'NONE', *, *, #508, .F. ) ;
#325 = CARTESIAN_POINT ( 'NONE',  ( 31.00000000000000000, 2.900000000000000355, -3.399999999999999911 ) ) ;
#326 = CIRCLE ( 'NONE', #9338, 2.500000000000000000 ) ;
#327 = CIRCLE ( 'NONE', #13072, 14.25000000000000000 ) ;
#328 = ORIENTED_EDGE ( 'NONE', *, *, #3752, .F. ) ;
#329 = CARTESIAN_POINT ( 'NONE',  ( 2.720000000000001528, 2.000000000000000000, 7.500000000000000888 ) ) ;
#330 = DIRECTION ( 'NONE',  ( -0.000000000000000000, -1.000000000000000000, -0.000000000000000000 ) ) ;
#331 = FACE_OUTER_BOUND ( 'NONE', #928, .T. ) ;
#332 = PLANE ( 'NONE',  #905 ) ;
#333 = CARTESIAN_POINT ( 'NONE',  ( 10.67828022838850366, 0.000000000000000000, -7.077546079049271022 ) ) ;
#334 = VECTOR ( 'NONE', #12084, 1000.000000000000000 ) ;
#335 = CARTESIAN_POINT ( 'NONE',  ( -8.914835885878215294, 0.000000000000000000, 11.11702303352197063 ) ) ;
#336 = TOROIDAL_SURFACE ( 'NONE', #2968, 3.100000000000000533, 0.1000000000000000056 ) ;
#337 = DIRECTION ( 'NONE',  ( -0.000000000000000000, -1.000000000000000000, -0.000000000000000000 ) ) ;
#338 = CARTESIAN_POINT ( 'NONE',  ( 0.000000000000000000, 9.000000000000000000, 0.000000000000000000 ) ) ;
#339 = ORIENTED_EDGE ( 'NONE', *, *, #792, .F. ) ;
#340 = ORIENTED_EDGE ( 'NONE', *, *, #11404, .T. ) ;
#341 = ORIENTED_EDGE ( 'NONE', *, *, #9398, .F. ) ;
#342 = ORIENTED_EDGE ( 'NONE', *, *, #5264, .T. ) ;
#343 = DIRECTION ( 'NONE',  ( 0.000000000000000000, 1.000000000000000000, -0.000000000000000000 ) ) ;
#344 = VERTEX_POINT ( 'NONE', #5616 ) ;
#345 = AXIS2_PLACEMENT_3D ( 'NONE', #12872, #1435, #8649 ) ;
#346 = EDGE_CURVE ( 'NONE', #9464, #11924, #3340, .T. ) ;
#347 = CARTESIAN_POINT ( 'NONE',  ( -8.369528376005813897, 9.000000000000000000, 1.483574994138650460 ) ) ;
#348 =( NAMED_UNIT ( * ) PLANE_ANGLE_UNIT ( ) SI_UNIT ( $, .RADIAN. ) );
#349 = CARTESIAN_POINT ( 'NONE',  ( 5.733772933379474246, 3.000000000000000000, -13.04554897075799502 ) ) ;
#350 = CARTESIAN_POINT ( 'NONE',  ( 28.47439151394123158, 3.000000000000000000, -2.423076923076924682 ) ) ;
#351 = B_SPLINE_SURFACE_WITH_KNOTS ( 'NONE', 3, 1, ( 
 ( #13128, #5749 ),
 ( #9949, #12175 ),
 ( #2724, #6930 ),
 ( #3542, #2648 ) ),
 .UNSPECIFIED., .F., .F., .F.,
 ( 4, 4 ),
 ( 2, 2 ),
 ( 0.000000000000000000, 0.8452273900860258760 ),
 ( 0.000000000000000000, 1.000000000000000000 ),
 .UNSPECIFIED. ) ;
#352 = DIRECTION ( 'NONE',  ( 0.000000000000000000, 1.000000000000000000, -0.000000000000000000 ) ) ;
#353 = EDGE_LOOP ( 'NONE', ( #2242, #11161, #428, #11636 ) ) ;
#354 = AXIS2_PLACEMENT_3D ( 'NONE', #12119, #12408, #12333 ) ;
#355 = DIRECTION ( 'NONE',  ( -0.000000000000000000, -1.000000000000000000, -0.000000000000000000 ) ) ;
#356 = ORIENTED_EDGE ( 'NONE', *, *, #4337, .T. ) ;
#357 = VERTEX_POINT ( 'NONE', #3539 ) ;
#358 = UNCERTAINTY_MEASURE_WITH_UNIT (LENGTH_MEASURE( 1.000000000000000082E-05 ), #5230, 'distance_accuracy_value', 'NONE');
#359 = ORIENTED_EDGE ( 'NONE', *, *, #9429, .F. ) ;
#360 = LINE ( 'NONE', #3375, #1597 ) ;
#361 = ORIENTED_EDGE ( 'NONE', *, *, #12415, .F. ) ;
#362 = EDGE_CURVE ( 'NONE', #1968, #1088, #10282, .T. ) ;
#363 = EDGE_LOOP ( 'NONE', ( #4629, #4721, #6765, #6549 ) ) ;
#364 = EDGE_CURVE ( 'NONE', #8366, #10838, #2983, .T. ) ;
#365 = CYLINDRICAL_SURFACE ( 'NONE', #13589, 8.500000000000000000 ) ;
#366 = DIRECTION ( 'NONE',  ( 0.000000000000000000, 0.000000000000000000, -1.000000000000000000 ) ) ;
#367 = ADVANCED_FACE ( 'NONE', ( #10218 ), #11113, .T. ) ;
#368 = CYLINDRICAL_SURFACE ( 'NONE', #6691, 6.749999999999999112 ) ;
#369 = ADVANCED_FACE ( 'NONE', ( #11247 ), #1681, .T. ) ;
#370 = CARTESIAN_POINT ( 'NONE',  ( 11.11702303352194043, 3.000000000000000000, -8.914835885878249044 ) ) ;
#371 = DIRECTION ( 'NONE',  ( 0.000000000000000000, 0.000000000000000000, 1.000000000000000000 ) ) ;
#372 = ORIENTED_EDGE ( 'NONE', *, *, #1521, .T. ) ;
#373 = CARTESIAN_POINT ( 'NONE',  ( 5.504794476853524188, 9.000000000000000000, -4.890042597913815570 ) ) ;
#374 = ORIENTED_EDGE ( 'NONE', *, *, #11346, .F. ) ;
#375 = VERTEX_POINT ( 'NONE', #9174 ) ;
#377 = ORIENTED_EDGE ( 'NONE', *, *, #9624, .T. ) ;
#376 = B_SPLINE_CURVE_WITH_KNOTS ( 'NONE', 2,
 ( #858, #13396, #4783 ),
 .UNSPECIFIED., .F., .F.,
 ( 3, 3 ),
 ( 0.000000000000000000, 1.000000000000000000 ),
 .UNSPECIFIED. ) ;
#378 = CARTESIAN_POINT ( 'NONE',  ( -8.479748006907131597, 0.000000000000000000, 0.5864074857593127854 ) ) ;
#379 = FACE_OUTER_BOUND ( 'NONE', #4363, .T. ) ;
#380 = CARTESIAN_POINT ( 'NONE',  ( -7.144272221052618832, 0.000000000000000000, 1.784003156764502940 ) ) ;
#381 = CARTESIAN_POINT ( 'NONE',  ( 12.21000000000000796, 3.000000000000000000, 0.2208617994340217328 ) ) ;
#382 = CARTESIAN_POINT ( 'NONE',  ( 0.000000000000000000, 0.000000000000000000, 3.400000000000001243 ) ) ;
#383 = DIRECTION ( 'NONE',  ( 0.000000000000000000, 0.000000000000000000, -1.000000000000000000 ) ) ;
#384 = ORIENTED_EDGE ( 'NONE', *, *, #10954, .T. ) ;
#385 = ORIENTED_EDGE ( 'NONE', *, *, #12086, .T. ) ;
#386 = CARTESIAN_POINT ( 'NONE',  ( -2.655466033450426533, 9.000000000000000000, -7.485541762018160128 ) ) ;
#387 = B_SPLINE_SURFACE_WITH_KNOTS ( 'NONE', 3, 1, ( 
 ( #6060, #3979 ),
 ( #1786, #3020 ),
 ( #2059, #9286 ),
 ( #760, #7090 ) ),
 .UNSPECIFIED., .F., .F., .F.,
 ( 4, 4 ),
 ( 2, 2 ),
 ( 0.000000000000000000, 0.8452273900860258760 ),
 ( 0.000000000000000000, 1.000000000000000000 ),
 .UNSPECIFIED. ) ;
#388 = EDGE_CURVE ( 'NONE', #9987, #6903, #13386, .T. ) ;
#389 = ORIENTED_EDGE ( 'NONE', *, *, #7985, .T. ) ;
#390 = CARTESIAN_POINT ( 'NONE',  ( 7.494008246337245716, 3.000000000000000000, -11.63517940784380578 ) ) ;
#391 = CARTESIAN_POINT ( 'NONE',  ( -14.90895795148409420, 0.000000000000000000, 1.650143266773909101 ) ) ;
#392 = DIRECTION ( 'NONE',  ( 0.000000000000000000, 0.000000000000000000, 1.000000000000000000 ) ) ;
#393 = CARTESIAN_POINT ( 'NONE',  ( -12.78643498603817896, 0.000000000000000000, 0.7901945867173603144 ) ) ;
#394 = LINE ( 'NONE', #9622, #244 ) ;
#395 = CARTESIAN_POINT ( 'NONE',  ( -8.180229652970899323, 3.000000000000000000, -11.90209577080756276 ) ) ;
#396 = FACE_BOUND ( 'NONE', #8897, .T. ) ;
#397 = CARTESIAN_POINT ( 'NONE',  ( -4.564691384634503635, 0.000000000000000000, 12.76342233970727769 ) ) ;
#398 = EDGE_LOOP ( 'NONE', ( #7206, #12127, #10777, #6516 ) ) ;
#399 = ORIENTED_EDGE ( 'NONE', *, *, #5721, .T. ) ;
#400 = ORIENTED_EDGE ( 'NONE', *, *, #9698, .F. ) ;
#401 = ORIENTED_EDGE ( 'NONE', *, *, #13079, .T. ) ;
#402 = DIRECTION ( 'NONE',  ( 0.000000000000000000, 0.000000000000000000, 1.000000000000000000 ) ) ;
#403 = ORIENTED_EDGE ( 'NONE', *, *, #2950, .F. ) ;
#404 = DIRECTION ( 'NONE',  ( 0.000000000000000000, 0.000000000000000000, -1.000000000000000000 ) ) ;
#405 = FACE_OUTER_BOUND ( 'NONE', #6501, .T. ) ;
#406 = B_SPLINE_CURVE_WITH_KNOTS ( 'NONE', 3,
 ( #3245, #11729, #7457, #5514 ),
 .UNSPECIFIED., .F., .F.,
 ( 4, 4 ),
 ( 0.1818127957067485756, 0.2112308727645026418 ),
 .UNSPECIFIED. ) ;
#407 = CARTESIAN_POINT ( 'NONE',  ( -5.065227977808753224, 9.000000000000000000, -4.461610195077944319 ) ) ;
#408 = CARTESIAN_POINT ( 'NONE',  ( 8.760376775873721655, 3.000000000000000000, -10.34346111134700585 ) ) ;
#409 = FACE_OUTER_BOUND ( 'NONE', #1971, .T. ) ;
#410 = ORIENTED_EDGE ( 'NONE', *, *, #2346, .T. ) ;
#411 = DIRECTION ( 'NONE',  ( -0.000000000000000000, -1.000000000000000000, -0.000000000000000000 ) ) ;
#412 = ORIENTED_EDGE ( 'NONE', *, *, #9690, .F. ) ;
#413 = EDGE_CURVE ( 'NONE', #5612, #7910, #10086, .T. ) ;
#414 = ORIENTED_EDGE ( 'NONE', *, *, #8684, .F. ) ;
#415 = LINE ( 'NONE', #13021, #10839 ) ;
#416 = ORIENTED_EDGE ( 'NONE', *, *, #2484, .T. ) ;
#417 = ORIENTED_EDGE ( 'NONE', *, *, #1401, .T. ) ;
#418 = AXIS2_PLACEMENT_3D ( 'NONE', #13510, #5924, #10269 ) ;
#419 = CARTESIAN_POINT ( 'NONE',  ( -14.90895795148411374, 0.000000000000000000, -1.650143266773683726 ) ) ;
#420 = CARTESIAN_POINT ( 'NONE',  ( 2.720000000000001528, 0.000000000000000000, 4.500000000000000000 ) ) ;
#421 = CARTESIAN_POINT ( 'NONE',  ( 0.8327827707325452522, 0.000000000000000000, 6.698430626405787791 ) ) ;
#422 = CARTESIAN_POINT ( 'NONE',  ( -5.452638258930639914, 3.000000000000000000, -13.97385902380748313 ) ) ;
#423 = CARTESIAN_POINT ( 'NONE',  ( -13.52637830886122572, 0.000000000000000000, -2.928250210355275218 ) ) ;
#424 = CARTESIAN_POINT ( 'NONE',  ( 50.46378962010818015, 3.000000000000000000, -4.178819016005276943 ) ) ;
#425 = ORIENTED_EDGE ( 'NONE', *, *, #11861, .F. ) ;
#426 = FACE_OUTER_BOUND ( 'NONE', #10907, .T. ) ;
#427 = EDGE_CURVE ( 'NONE', #11681, #3761, #12365, .T. ) ;
#428 = ORIENTED_EDGE ( 'NONE', *, *, #6747, .F. ) ;
#429 = ADVANCED_FACE ( 'NONE', ( #4581 ), #2651, .F. ) ;
#430 = ORIENTED_EDGE ( 'NONE', *, *, #1575, .F. ) ;
#431 = EDGE_LOOP ( 'NONE', ( #8073, #1131 ) ) ;
#432 = EDGE_CURVE ( 'NONE', #1362, #2254, #9941, .T. ) ;
#433 = ADVANCED_FACE ( 'NONE', ( #4281 ), #6408, .T. ) ;
#434 = VECTOR ( 'NONE', #1224, 1000.000000000000000 ) ;
#435 = CARTESIAN_POINT ( 'NONE',  ( 20.00000000000000711, 0.000000000000000000, 12.57924256039204280 ) ) ;
#436 = CARTESIAN_POINT ( 'NONE',  ( 31.00000000000000000, 3.000000000000000000, 3.999999998926329514 ) ) ;
#437 = DIRECTION ( 'NONE',  ( 0.6291930273683107311, 0.000000000000000000, -0.7772490812545873595 ) ) ;
#438 = CARTESIAN_POINT ( 'NONE',  ( 12.63269908545826503, 0.000000000000000000, -5.340493616518843467 ) ) ;
#439 = CARTESIAN_POINT ( 'NONE',  ( 7.363612555047485131, 0.000000000000000000, -0.02242701489043354146 ) ) ;
#440 = LINE ( 'NONE', #7672, #4428 ) ;
#441 = DIRECTION ( 'NONE',  ( 0.000000000000000000, 0.000000000000000000, 1.000000000000000000 ) ) ;
#442 = DIRECTION ( 'NONE',  ( -0.000000000000000000, -1.000000000000000000, -0.000000000000000000 ) ) ;
#443 = AXIS2_PLACEMENT_3D ( 'NONE', #4842, #10911, #11044 ) ;
#444 = EDGE_CURVE ( 'NONE', #11209, #5642, #3242, .T. ) ;
#445 = MECHANICAL_DESIGN_GEOMETRIC_PRESENTATION_REPRESENTATION (  '', ( #6386 ), #6171 ) ;
#446 = ORIENTED_EDGE ( 'NONE', *, *, #6514, .F. ) ;
#447 = VERTEX_POINT ( 'NONE', #8333 ) ;
#448 = EDGE_CURVE ( 'NONE', #3825, #117, #4011, .T. ) ;
#449 = ORIENTED_EDGE ( 'NONE', *, *, #5832, .F. ) ;
#450 = CARTESIAN_POINT ( 'NONE',  ( 0.000000000000000000, 0.000000000000000000, 0.000000000000000000 ) ) ;
#451 = CARTESIAN_POINT ( 'NONE',  ( 0.000000000000000000, 9.000000000000000000, 0.000000000000000000 ) ) ;
#452 = CIRCLE ( 'NONE', #7929, 5.499999999999996447 ) ;
#453 = VECTOR ( 'NONE', #9150, 1000.000000000000000 ) ;
#454 = DIRECTION ( 'NONE',  ( 0.000000000000000000, 0.000000000000000000, 1.000000000000000000 ) ) ;
#455 = DIRECTION ( 'NONE',  ( 0.000000000000000000, 1.000000000000000000, -0.000000000000000000 ) ) ;
#456 = LINE ( 'NONE', #4526, #902 ) ;
#457 = LINE ( 'NONE', #7759, #5366 ) ;
#458 = EDGE_CURVE ( 'NONE', #7779, #12211, #11592, .T. ) ;
#459 = FACE_OUTER_BOUND ( 'NONE', #9234, .T. ) ;
#460 = EDGE_CURVE ( 'NONE', #8976, #10417, #11713, .T. ) ;
#461 = LINE ( 'NONE', #5837, #521 ) ;
#462 = ORIENTED_EDGE ( 'NONE', *, *, #10785, .F. ) ;
#463 = CIRCLE ( 'NONE', #3104, 5.486375544325371223 ) ;
#464 = VERTEX_POINT ( 'NONE', #3179 ) ;
#465 = AXIS2_PLACEMENT_3D ( 'NONE', #7088, #12335, #6953 ) ;
#466 = ORIENTED_EDGE ( 'NONE', *, *, #3127, .F. ) ;
#467 = ORIENTED_EDGE ( 'NONE', *, *, #12897, .T. ) ;
#468 = CARTESIAN_POINT ( 'NONE',  ( -0.1834773636644435324, 0.000000000000000000, -13.00394737445024873 ) ) ;
#469 = ORIENTED_EDGE ( 'NONE', *, *, #9034, .T. ) ;
#470 = LINE ( 'NONE', #8726, #4829 ) ;
#471 = VECTOR ( 'NONE', #5300, 1000.000000000000000 ) ;
#472 = CARTESIAN_POINT ( 'NONE',  ( 12.21000000000000796, 3.000000000000000000, 0.2208617994340217328 ) ) ;
#473 = CARTESIAN_POINT ( 'NONE',  ( 6.017756925049591921, 3.000000000000000000, -11.52330688609011844 ) ) ;
#474 = LINE ( 'NONE', #4679, #13306 ) ;
#475 = CARTESIAN_POINT ( 'NONE',  ( 0.000000000000000000, 3.000000000000000000, 0.000000000000000000 ) ) ;
#476 = DIRECTION ( 'NONE',  ( 0.000000000000000000, 0.000000000000000000, -1.000000000000000000 ) ) ;
#477 = ORIENTED_EDGE ( 'NONE', *, *, #3906, .F. ) ;
#478 = CARTESIAN_POINT ( 'NONE',  ( 0.000000000000000000, 3.000000000000000000, 0.000000000000000000 ) ) ;
#479 = VERTEX_POINT ( 'NONE', #12756 ) ;
#480 = UNCERTAINTY_MEASURE_WITH_UNIT (LENGTH_MEASURE( 1.000000000000000082E-05 ), #13297, 'distance_accuracy_value', 'NONE');
#481 = CIRCLE ( 'NONE', #6643, 0.1000000000000000472 ) ;
#482 = EDGE_LOOP ( 'NONE', ( #4350, #4366, #12937, #9187 ) ) ;
#483 = CARTESIAN_POINT ( 'NONE',  ( -13.00394681030572208, 3.000000000000000000, -0.1834665838397169235 ) ) ;
#484 = CIRCLE ( 'NONE', #8176, 12.08999999999737440 ) ;
#485 = ORIENTED_EDGE ( 'NONE', *, *, #6813, .T. ) ;
#486 = ORIENTED_EDGE ( 'NONE', *, *, #11722, .T. ) ;
#487 = DIRECTION ( 'NONE',  ( -0.000000000000000000, -1.000000000000000000, -0.000000000000000000 ) ) ;
#488 = LINE ( 'NONE', #2617, #1153 ) ;
#489 =( NAMED_UNIT ( * ) SI_UNIT ( $, .STERADIAN. ) SOLID_ANGLE_UNIT ( ) );
#490 = EDGE_CURVE ( 'NONE', #10298, #5890, #7389, .T. ) ;
#491 = AXIS2_PLACEMENT_3D ( 'NONE', #848, #12295, #6081 ) ;
#492 = CARTESIAN_POINT ( 'NONE',  ( -2.830255545554292151, 3.000000000000000000, -12.68816982652971959 ) ) ;
#493 = CIRCLE ( 'NONE', #9944, 3.399999999999999911 ) ;
#494 = CIRCLE ( 'NONE', #3132, 2.500000000000000444 ) ;
#495 = CARTESIAN_POINT ( 'NONE',  ( -12.25836857253663759, 0.000000000000000000, -5.784789447945487773 ) ) ;
#496 = CARTESIAN_POINT ( 'NONE',  ( 13.27898586450067242, 0.000000000000000000, -5.170206418547655502 ) ) ;
#497 = ORIENTED_EDGE ( 'NONE', *, *, #9087, .T. ) ;
#498 = CARTESIAN_POINT ( 'NONE',  ( 0.000000000000000000, 0.000000000000000000, 5.000000000000000000 ) ) ;
#499 = B_SPLINE_SURFACE_WITH_KNOTS ( 'NONE', 3, 1, ( 
 ( #6298, #5461 ),
 ( #3400, #5208 ),
 ( #10510, #11814 ),
 ( #1268, #10711 ) ),
 .UNSPECIFIED., .F., .F., .F.,
 ( 4, 4 ),
 ( 2, 2 ),
 ( 0.000000000000000000, 0.5855695330273008592 ),
 ( 0.000000000000000000, 1.000000000000000000 ),
 .UNSPECIFIED. ) ;
#500 = VERTEX_POINT ( 'NONE', #11383 ) ;
#501 = ORIENTED_EDGE ( 'NONE', *, *, #4582, .F. ) ;
#502 = ORIENTED_EDGE ( 'NONE', *, *, #9169, .T. ) ;
#503 = AXIS2_PLACEMENT_3D ( 'NONE', #11418, #6309, #4045 ) ;
#504 = AXIS2_PLACEMENT_3D ( 'NONE', #4653, #13064, #10988 ) ;
#505 = COLOUR_RGB ( '',0.7803921568627451011, 0.7607843137254901578, 0.7411764705882353255 ) ;
#506 = CARTESIAN_POINT ( 'NONE',  ( -13.49999999999999645, 0.000000000000000000, -8.549999999999998934 ) ) ;
#507 = DIRECTION ( 'NONE',  ( 0.000000000000000000, 0.000000000000000000, 1.000000000000000000 ) ) ;
#508 = EDGE_CURVE ( 'NONE', #12112, #12067, #13480, .T. ) ;
#509 = CARTESIAN_POINT ( 'NONE',  ( -13.33579367773357482, 0.000000000000000000, 2.428572470324200427 ) ) ;
#510 = EDGE_CURVE ( 'NONE', #12325, #8354, #13389, .T. ) ;
#511 = CARTESIAN_POINT ( 'NONE',  ( -0.5501230721523990841, 0.000000000000000000, -12.98835496148299384 ) ) ;
#512 = CONTEXT_DEPENDENT_SHAPE_REPRESENTATION ( #7483, #88 ) ;
#513 = CARTESIAN_POINT ( 'NONE',  ( 8.883544964651964193, 3.000000000000000000, -12.08646469655236544 ) ) ;
#514 = CARTESIAN_POINT ( 'NONE',  ( 0.000000000000000000, 9.000000000000000000, 0.000000000000000000 ) ) ;
#515 = CARTESIAN_POINT ( 'NONE',  ( 22.00000000000000000, 0.000000000000000000, 0.000000000000000000 ) ) ;
#516 = AXIS2_PLACEMENT_3D ( 'NONE', #8094, #8227, #869 ) ;
#517 = DIRECTION ( 'NONE',  ( -0.000000000000000000, -1.000000000000000000, -0.000000000000000000 ) ) ;
#518 = CARTESIAN_POINT ( 'NONE',  ( 0.000000000000000000, 9.000000000000000000, 0.000000000000000000 ) ) ;
#519 = VECTOR ( 'NONE', #1899, 1000.000000000000000 ) ;
#520 = ADVANCED_FACE ( 'NONE', ( #5381 ), #8916, .F. ) ;
#521 = VECTOR ( 'NONE', #5626, 1000.000000000000000 ) ;
#522 = B_SPLINE_CURVE_WITH_KNOTS ( 'NONE', 3,
 ( #12540, #2883, #11494, #4182 ),
 .UNSPECIFIED., .F., .F.,
 ( 4, 4 ),
 ( 0.000000000000000000, 0.5855695330273008592 ),
 .UNSPECIFIED. ) ;
#523 = VERTEX_POINT ( 'NONE', #12504 ) ;
#524 = ORIENTED_EDGE ( 'NONE', *, *, #7234, .T. ) ;
#525 = VERTEX_POINT ( 'NONE', #8535 ) ;
#526 = DIRECTION ( 'NONE',  ( -0.000000000000000000, -1.000000000000000000, -0.000000000000000000 ) ) ;
#527 = VECTOR ( 'NONE', #5207, 1000.000000000000000 ) ;
#528 = PRODUCT ( 'base-plate', 'base-plate', '', ( #2121 ) ) ;
#529 = AXIS2_PLACEMENT_3D ( 'NONE', #3588, #12216, #3653 ) ;
#530 = PLANE ( 'NONE',  #9767 ) ;
#531 = EDGE_CURVE ( 'NONE', #8124, #10022, #4668, .T. ) ;
#532 = CARTESIAN_POINT ( 'NONE',  ( 19.65244806805498357, 3.000000000000000000, -6.000000000000000000 ) ) ;
#533 = CARTESIAN_POINT ( 'NONE',  ( 4.652003457867571967, 9.000000000000000000, -6.437678087145717321 ) ) ;
#534 = CARTESIAN_POINT ( 'NONE',  ( 20.03271148078819408, 3.000000000000000000, -5.075121771833452478 ) ) ;
#535 = EDGE_CURVE ( 'NONE', #8580, #8655, #4009, .T. ) ;
#536 = CARTESIAN_POINT ( 'NONE',  ( -11.90209577080766046, 3.000000000000000000, -8.180229652970757215 ) ) ;
#537 = ADVANCED_FACE ( 'NONE', ( #23 ), #13587, .F. ) ;
#538 = DIRECTION ( 'NONE',  ( 8.881784197001252323E-16, 0.000000000000000000, 1.000000000000000000 ) ) ;
#539 = AXIS2_PLACEMENT_3D ( 'NONE', #2331, #9566, #7561 ) ;
#540 = DIRECTION ( 'NONE',  ( 0.000000000000000000, 1.000000000000000000, -0.000000000000000000 ) ) ;
#541 = AXIS2_PLACEMENT_3D ( 'NONE', #13133, #7884, #11067 ) ;
#542 = ORIENTED_EDGE ( 'NONE', *, *, #301, .T. ) ;
#543 = ORIENTED_EDGE ( 'NONE', *, *, #11120, .F. ) ;
#544 = VERTEX_POINT ( 'NONE', #6210 ) ;
#545 = CARTESIAN_POINT ( 'NONE',  ( -2.604399508763951321, 3.000000000000000000, 11.80615107470197422 ) ) ;
#546 = ORIENTED_EDGE ( 'NONE', *, *, #12833, .F. ) ;
#547 = CARTESIAN_POINT ( 'NONE',  ( 0.000000000000000000, 3.000000000000000000, 0.000000000000000000 ) ) ;
#548 = CIRCLE ( 'NONE', #5169, 1.500000000000003997 ) ;
#549 = DIRECTION ( 'NONE',  ( -0.3537595828326807190, 1.222174860403972347E-21, -0.9353363873783847593 ) ) ;
#550 = CIRCLE ( 'NONE', #6708, 12.08999999999737618 ) ;
#551 = DIRECTION ( 'NONE',  ( -0.000000000000000000, -1.000000000000000000, -0.000000000000000000 ) ) ;
#552 = DIRECTION ( 'NONE',  ( 0.000000000000000000, 0.000000000000000000, 1.000000000000000000 ) ) ;
#553 = CIRCLE ( 'NONE', #1211, 3.500000000000000888 ) ;
#554 = DIRECTION ( 'NONE',  ( 1.269138026879196405E-16, 0.000000000000000000, 1.000000000000000000 ) ) ;
#555 = DIRECTION ( 'NONE',  ( 0.000000000000000000, 0.000000000000000000, -1.000000000000000000 ) ) ;
#556 = CARTESIAN_POINT ( 'NONE',  ( -6.025412986832177076, 3.000000000000000000, -13.73660796332610268 ) ) ;
#557 = ORIENTED_EDGE ( 'NONE', *, *, #3167, .F. ) ;
#558 = CARTESIAN_POINT ( 'NONE',  ( 8.093005444143644311, 9.000000000000000000, -2.598704077239528232 ) ) ;
#559 = EDGE_LOOP ( 'NONE', ( #8381, #3710, #2080, #13458 ) ) ;
#560 = AXIS2_PLACEMENT_3D ( 'NONE', #3107, #4208, #10695 ) ;
#561 = EDGE_LOOP ( 'NONE', ( #2555, #11444 ) ) ;
#562 = AXIS2_PLACEMENT_3D ( 'NONE', #11848, #2406, #1375 ) ;
#563 = LINE ( 'NONE', #1798, #9730 ) ;
#564 = ORIENTED_EDGE ( 'NONE', *, *, #7340, .T. ) ;
#565 = EDGE_CURVE ( 'NONE', #13387, #8347, #11519, .T. ) ;
#566 = ORIENTED_EDGE ( 'NONE', *, *, #7660, .T. ) ;
#567 = ADVANCED_FACE ( 'NONE', ( #10952 ), #5726, .F. ) ;
#568 = CARTESIAN_POINT ( 'NONE',  ( -11.52330688609014686, 0.000000000000000000, -6.017756925049552841 ) ) ;
#569 = FILL_AREA_STYLE ('',( #9990 ) ) ;
#570 = FACE_OUTER_BOUND ( 'NONE', #4411, .T. ) ;
#571 = CARTESIAN_POINT ( 'NONE',  ( 1.557181465540758758, 3.000000000000000000, 14.16466328168009881 ) ) ;
#572 = CARTESIAN_POINT ( 'NONE',  ( 52.34174591811297717, 3.000000000000000000, -12.24483450274845531 ) ) ;
#573 = FACE_OUTER_BOUND ( 'NONE', #5707, .T. ) ;
#574 = CARTESIAN_POINT ( 'NONE',  ( 4.690415759823430619, 2.900000000000000355, -4.500000000000000888 ) ) ;
#575 = ORIENTED_EDGE ( 'NONE', *, *, #6812, .F. ) ;
#576 = CARTESIAN_POINT ( 'NONE',  ( 0.000000000000000000, 2.900000000000000355, 0.000000000000000000 ) ) ;
#577 = ORIENTED_EDGE ( 'NONE', *, *, #13185, .F. ) ;
#578 = VERTEX_POINT ( 'NONE', #7650 ) ;
#579 = B_SPLINE_SURFACE_WITH_KNOTS ( 'NONE', 3, 1, ( 
 ( #4760, #8946 ),
 ( #13160, #3708 ),
 ( #6886, #7909 ),
 ( #10120, #3025 ) ),
 .UNSPECIFIED., .F., .F., .F.,
 ( 4, 4 ),
 ( 2, 2 ),
 ( 0.000000000000000000, 0.8452273900860258760 ),
 ( 0.000000000000000000, 1.000000000000000000 ),
 .UNSPECIFIED. ) ;
#580 = ORIENTED_EDGE ( 'NONE', *, *, #11985, .T. ) ;
#581 = PRODUCT_DEFINITION_FORMATION_WITH_SPECIFIED_SOURCE ( 'ANY', '', #4340, .NOT_KNOWN. ) ;
#582 = B_SPLINE_CURVE_WITH_KNOTS ( 'NONE', 3,
 ( #1871, #5783, #10055, #4884 ),
 .UNSPECIFIED., .F., .F.,
 ( 4, 4 ),
 ( 0.000000000000000000, 0.8452273900860258760 ),
 .UNSPECIFIED. ) ;
#583 = CARTESIAN_POINT ( 'NONE',  ( 8.252687871541644071, 0.000000000000000000, 28.00000000000000000 ) ) ;
#584 = DIRECTION ( 'NONE',  ( 0.000000000000000000, 1.000000000000000000, 0.000000000000000000 ) ) ;
#585 = DIRECTION ( 'NONE',  ( 0.000000000000000000, 0.000000000000000000, 1.000000000000000000 ) ) ;
#586 = CARTESIAN_POINT ( 'NONE',  ( 5.967832595844251742, 0.000000000000000000, -3.153961652902404822 ) ) ;
#587 = LINE ( 'NONE', #922, #674 ) ;
#588 = ITEM_DEFINED_TRANSFORMATION ( 'NONE', 'NONE', #3198,  #10007 ) ;
#589 = FACE_OUTER_BOUND ( 'NONE', #13557, .T. ) ;
#590 = DIRECTION ( 'NONE',  ( 0.000000000000000000, 0.000000000000000000, 1.000000000000000000 ) ) ;
#591 = DIRECTION ( 'NONE',  ( -0.000000000000000000, -1.000000000000000000, -0.000000000000000000 ) ) ;
#592 = CARTESIAN_POINT ( 'NONE',  ( -3.893011711613112880, 0.000000000000000000, -12.40340517008282717 ) ) ;
#593 = CARTESIAN_POINT ( 'NONE',  ( 49.72134184781355515, 0.000000000000000000, -3.261665100124877981 ) ) ;
#594 = VERTEX_POINT ( 'NONE', #2556 ) ;
#595 = EDGE_LOOP ( 'NONE', ( #4853, #1217, #4392, #497, #6612, #11542, #2963, #3783 ) ) ;
#596 = EDGE_CURVE ( 'NONE', #2976, #3318, #5708, .T. ) ;
#597 = VERTEX_POINT ( 'NONE', #11720 ) ;
#598 = CARTESIAN_POINT ( 'NONE',  ( -21.21140389626389222, 0.000000000000000000, 12.49772878833445056 ) ) ;
#599 = FACE_OUTER_BOUND ( 'NONE', #1472, .T. ) ;
#600 = DIRECTION ( 'NONE',  ( 0.000000000000000000, 0.000000000000000000, 1.000000000000000000 ) ) ;
#601 = DIRECTION ( 'NONE',  ( 0.000000000000000000, 1.000000000000000000, 0.000000000000000000 ) ) ;
#602 = DIRECTION ( 'NONE',  ( -0.000000000000000000, -1.000000000000000000, -0.000000000000000000 ) ) ;
#603 = DIRECTION ( 'NONE',  ( 1.000000000000000000, -3.469446951953610639E-15, -2.602085213965210149E-16 ) ) ;
#604 = CARTESIAN_POINT ( 'NONE',  ( -12.68816982652970893, 3.000000000000000000, 2.830255545554337004 ) ) ;
#605 = CARTESIAN_POINT ( 'NONE',  ( -3.647470871583628593, 0.000000000000000000, 11.52666717836884125 ) ) ;
#606 = EDGE_LOOP ( 'NONE', ( #10674, #7647, #5644, #642 ) ) ;
#607 = EDGE_CURVE ( 'NONE', #10071, #5801, #415, .T. ) ;
#608 = ORIENTED_EDGE ( 'NONE', *, *, #6998, .F. ) ;
#609 = EDGE_CURVE ( 'NONE', #5612, #2261, #8875, .T. ) ;
#610 = ORIENTED_EDGE ( 'NONE', *, *, #4580, .T. ) ;
#611 = DIRECTION ( 'NONE',  ( -0.000000000000000000, -1.000000000000000000, -0.000000000000000000 ) ) ;
#612 = ORIENTED_EDGE ( 'NONE', *, *, #3358, .T. ) ;
#613 = EDGE_CURVE ( 'NONE', #1248, #75, #3577, .T. ) ;
#614 = ADVANCED_FACE ( 'NONE', ( #3441 ), #10691, .F. ) ;
#615 = DIRECTION ( 'NONE',  ( 0.000000000000000000, 1.000000000000000000, -0.000000000000000000 ) ) ;
#616 = CARTESIAN_POINT ( 'NONE',  ( 42.17696780345873009, 41.33135765298363395, 35.00042399991640707 ) ) ;
#617 = CARTESIAN_POINT ( 'NONE',  ( 0.000000000000000000, 0.000000000000000000, -1.500000000000000222 ) ) ;
#618 = CARTESIAN_POINT ( 'NONE',  ( 13.40069634612381044, 3.000000000000000000, 2.546644602219900300 ) ) ;
#619 = CARTESIAN_POINT ( 'NONE',  ( -6.506507307819711095, 0.000000000000000000, 10.18987059060247624 ) ) ;
#620 = CARTESIAN_POINT ( 'NONE',  ( 8.922226997226882617, 3.000000000000000000, 8.158551673544282679 ) ) ;
#621 = DIRECTION ( 'NONE',  ( 0.000000000000000000, 0.000000000000000000, 1.000000000000000000 ) ) ;
#622 = EDGE_LOOP ( 'NONE', ( #11651, #11442, #4299, #11608 ) ) ;
#623 = LINE ( 'NONE', #3704, #12180 ) ;
#624 = EDGE_CURVE ( 'NONE', #2462, #5247, #6615, .T. ) ;
#625 = ORIENTED_EDGE ( 'NONE', *, *, #2071, .F. ) ;
#626 = ORIENTED_EDGE ( 'NONE', *, *, #9282, .F. ) ;
#627 = CARTESIAN_POINT ( 'NONE',  ( -1.557181465540221188, 3.000000000000000000, 14.16466328168015743 ) ) ;
#628 = ORIENTED_EDGE ( 'NONE', *, *, #460, .T. ) ;
#629 = CARTESIAN_POINT ( 'NONE',  ( 12.08646469655232636, 3.000000000000000000, -8.883544964652022813 ) ) ;
#630 = ORIENTED_EDGE ( 'NONE', *, *, #11392, .T. ) ;
#631 = DIRECTION ( 'NONE',  ( 0.000000000000000000, 0.000000000000000000, -1.000000000000000000 ) ) ;
#632 = CARTESIAN_POINT ( 'NONE',  ( -6.329356821613726147, 3.000000000000000000, -12.30759122142001338 ) ) ;
#633 = CARTESIAN_POINT ( 'NONE',  ( -5.830003112347290184, 0.000000000000000000, -5.394061460138155795 ) ) ;
#634 = CARTESIAN_POINT ( 'NONE',  ( -12.38517345876401521, 3.000000000000000000, -12.42191571009144901 ) ) ;
#635 = CARTESIAN_POINT ( 'NONE',  ( -0.8148820470561124463, 0.000000000000000000, 6.700631854488474204 ) ) ;
#636 = CARTESIAN_POINT ( 'NONE',  ( 4.690415759823430619, 0.09999999999999982514, 4.500000000000000888 ) ) ;
#637 = ORIENTED_EDGE ( 'NONE', *, *, #10382, .F. ) ;
#638 = CARTESIAN_POINT ( 'NONE',  ( -5.784789447945489549, 3.000000000000000000, 12.25836857253663581 ) ) ;
#639 = ADVANCED_BREP_SHAPE_REPRESENTATION ( '', ( #3911, #10007 ), #12660 ) ;
#640 = ADVANCED_FACE ( 'NONE', ( #7783 ), #12001, .T. ) ;
#641 = VERTEX_POINT ( 'NONE', #2277 ) ;
#642 = ORIENTED_EDGE ( 'NONE', *, *, #49, .T. ) ;
#643 = DIRECTION ( 'NONE',  ( 0.000000000000000000, 0.000000000000000000, -1.000000000000000000 ) ) ;
#644 = ORIENTED_EDGE ( 'NONE', *, *, #13323, .T. ) ;
#645 = CARTESIAN_POINT ( 'NONE',  ( 31.00000000000000000, 3.000000000000000000, 0.000000000000000000 ) ) ;
#646 = DIRECTION ( 'NONE',  ( -0.7772490812545873595, 0.000000000000000000, -0.6291930273683107311 ) ) ;
#647 = CARTESIAN_POINT ( 'NONE',  ( 0.000000000000000000, 9.000000000000000000, 0.000000000000000000 ) ) ;
#648 = DIRECTION ( 'NONE',  ( -3.469446951953614189E-15, -1.000000000000000000, 8.673617379884035472E-16 ) ) ;
#649 = CONTEXT_DEPENDENT_SHAPE_REPRESENTATION ( #8360, #2266 ) ;
#650 = CARTESIAN_POINT ( 'NONE',  ( 8.373678438139048552, 9.000000000000000000, 1.459968977288628178 ) ) ;
#651 = CARTESIAN_POINT ( 'NONE',  ( -7.723663868796776910, 3.000000000000000000, -11.13895890373326303 ) ) ;
#652 = CARTESIAN_POINT ( 'NONE',  ( 2.604399508763944660, 3.000000000000000000, -11.80615107470197600 ) ) ;
#653 = CARTESIAN_POINT ( 'NONE',  ( -5.170206418547658167, 0.000000000000000000, -13.27898586450066887 ) ) ;
#654 = CARTESIAN_POINT ( 'NONE',  ( -3.647599401157691545, 3.000000000000000000, -11.52662650599084238 ) ) ;
#655 = VERTEX_POINT ( 'NONE', #11922 ) ;
#656 = ORIENTED_EDGE ( 'NONE', *, *, #9257, .F. ) ;
#657 = VECTOR ( 'NONE', #1576, 1000.000000000000000 ) ;
#658 = ORIENTED_EDGE ( 'NONE', *, *, #13257, .F. ) ;
#659 = CARTESIAN_POINT ( 'NONE',  ( -8.158551673544284455, 3.000000000000000000, 8.922226997226891498 ) ) ;
#660 = FACE_OUTER_BOUND ( 'NONE', #10677, .T. ) ;
#661 = DIRECTION ( 'NONE',  ( 0.000000000000000000, 0.000000000000000000, 1.000000000000000000 ) ) ;
#662 = AXIS2_PLACEMENT_3D ( 'NONE', #2861, #601, #2728 ) ;
#663 = CYLINDRICAL_SURFACE ( 'NONE', #1571, 6.749999999999999112 ) ;
#664 = DIRECTION ( 'NONE',  ( 0.9248782281665489657, 0.000000000000000000, -0.3802634127332067404 ) ) ;
#665 = AXIS2_PLACEMENT_3D ( 'NONE', #9357, #12667, #2244 ) ;
#666 = EDGE_CURVE ( 'NONE', #1008, #7348, #6486, .T. ) ;
#667 = CARTESIAN_POINT ( 'NONE',  ( 7.248474140376191421, 9.000000000000000000, 4.439552076088042476 ) ) ;
#668 = DIRECTION ( 'NONE',  ( 0.000000000000000000, 0.000000000000000000, -1.000000000000000000 ) ) ;
#669 = CARTESIAN_POINT ( 'NONE',  ( -4.056222772158361245, 0.000000000000000000, 12.16218796965919324 ) ) ;
#670 = ORIENTED_EDGE ( 'NONE', *, *, #4159, .T. ) ;
#671 = ORIENTED_EDGE ( 'NONE', *, *, #13142, .F. ) ;
#672 = VERTEX_POINT ( 'NONE', #12826 ) ;
#673 = CARTESIAN_POINT ( 'NONE',  ( -2.414978278956346092, 0.000000000000000000, 13.33788847341978467 ) ) ;
#674 = VECTOR ( 'NONE', #7131, 1000.000000000000000 ) ;
#675 = ORIENTED_EDGE ( 'NONE', *, *, #4510, .T. ) ;
#676 = DIRECTION ( 'NONE',  ( 0.000000000000000000, 0.000000000000000000, 1.000000000000000000 ) ) ;
#677 = DIRECTION ( 'NONE',  ( 0.000000000000000000, 0.000000000000000000, 1.000000000000000000 ) ) ;
#678 = EDGE_CURVE ( 'NONE', #6263, #3116, #360, .T. ) ;
#679 = DIRECTION ( 'NONE',  ( -0.000000000000000000, -1.000000000000000000, -0.000000000000000000 ) ) ;
#680 = CARTESIAN_POINT ( 'NONE',  ( 6.506507307819716424, 3.000000000000000000, -10.18987059060247269 ) ) ;
#681 = EDGE_CURVE ( 'NONE', #2253, #3491, #9506, .T. ) ;
#682 = CIRCLE ( 'NONE', #5520, 12.08999999999737440 ) ;
#683 = CARTESIAN_POINT ( 'NONE',  ( 0.000000000000000000, 0.000000000000000000, 0.000000000000000000 ) ) ;
#684 = CIRCLE ( 'NONE', #8370, 12.08999999999737263 ) ;
#685 = CARTESIAN_POINT ( 'NONE',  ( 28.47439151394123158, 2.900000000000000355, 2.423076923076924238 ) ) ;
#686 = AXIS2_PLACEMENT_3D ( 'NONE', #5417, #1154, #13562 ) ;
#687 = LINE ( 'NONE', #5850, #12010 ) ;
#688 = VERTEX_POINT ( 'NONE', #10752 ) ;
#689 = CARTESIAN_POINT ( 'NONE',  ( 0.000000000000000000, 3.000000000000000000, 0.000000000000000000 ) ) ;
#690 = EDGE_CURVE ( 'NONE', #9707, #1933, #9292, .T. ) ;
#691 = ORIENTED_EDGE ( 'NONE', *, *, #2431, .T. ) ;
#692 = VERTEX_POINT ( 'NONE', #11854 ) ;
#693 = CARTESIAN_POINT ( 'NONE',  ( 6.329356821613516537, 3.000000000000000000, -12.30759122141987305 ) ) ;
#694 = ORIENTED_EDGE ( 'NONE', *, *, #5265, .T. ) ;
#695 = CARTESIAN_POINT ( 'NONE',  ( 3.893011711613070691, 0.000000000000000000, -12.40340517008307231 ) ) ;
#696 = AXIS2_PLACEMENT_3D ( 'NONE', #10163, #9957, #13351 ) ;
#697 = ORIENTED_EDGE ( 'NONE', *, *, #1747, .T. ) ;
#698 = DIRECTION ( 'NONE',  ( 0.000000000000000000, 1.000000000000000000, -0.000000000000000000 ) ) ;
#699 = CARTESIAN_POINT ( 'NONE',  ( 30.82048254704846713, 0.000000000000000000, -7.998976482636475538 ) ) ;
#700 = ADVANCED_FACE ( 'NONE', ( #10889 ), #9711, .F. ) ;
#701 = LINE ( 'NONE', #3093, #9681 ) ;
#702 = FACE_OUTER_BOUND ( 'NONE', #12220, .T. ) ;
#703 = CARTESIAN_POINT ( 'NONE',  ( -5.526615004551211463, 0.000000000000000000, -4.866191470063547797 ) ) ;
#704 = DIRECTION ( 'NONE',  ( 0.000000000000000000, 0.000000000000000000, -1.000000000000000000 ) ) ;
#705 = ORIENTED_EDGE ( 'NONE', *, *, #2472, .T. ) ;
#706 = LINE ( 'NONE', #11030, #6217 ) ;
#707 = EDGE_CURVE ( 'NONE', #8736, #9662, #5546, .T. ) ;
#708 = AXIS2_PLACEMENT_3D ( 'NONE', #11662, #2221, #6424 ) ;
#709 = ORIENTED_EDGE ( 'NONE', *, *, #2346, .F. ) ;
#710 = VERTEX_POINT ( 'NONE', #10194 ) ;
#711 = DIRECTION ( 'NONE',  ( -0.000000000000000000, -1.000000000000000000, -0.000000000000000000 ) ) ;
#712 = ORIENTED_EDGE ( 'NONE', *, *, #9478, .F. ) ;
#713 = APPLICATION_CONTEXT ( 'automotive_design' ) ;
#714 = CARTESIAN_POINT ( 'NONE',  ( 8.771102293099069414, 0.000000000000000000, 10.33484986938308303 ) ) ;
#715 = SURFACE_STYLE_USAGE ( .BOTH. , #6144 ) ;
#716 = CIRCLE ( 'NONE', #13481, 5.486375544325371223 ) ;
#717 = VECTOR ( 'NONE', #10109, 1000.000000000000000 ) ;
#718 = CARTESIAN_POINT ( 'NONE',  ( 0.000000000000000000, 0.000000000000000000, 0.000000000000000000 ) ) ;
#719 = CARTESIAN_POINT ( 'NONE',  ( -13.04554897075796127, 0.000000000000000000, 5.733772933379547077 ) ) ;
#720 = EDGE_CURVE ( 'NONE', #5890, #9922, #3343, .T. ) ;
#721 = CARTESIAN_POINT ( 'NONE',  ( -0.6724118135763151871, 0.000000000000000000, -13.82336506795071784 ) ) ;
#722 = DIRECTION ( 'NONE',  ( 1.000000000000000000, 0.000000000000000000, 0.000000000000000000 ) ) ;
#723 = CARTESIAN_POINT ( 'NONE',  ( -5.299649803506881085, 0.000000000000000000, -6.645578376649351249 ) ) ;
#724 = PLANE ( 'NONE',  #1129 ) ;
#725 = CYLINDRICAL_SURFACE ( 'NONE', #10420, 2.999999999999999112 ) ;
#726 = CYLINDRICAL_SURFACE ( 'NONE', #3574, 1.500000000000001332 ) ;
#727 = ORIENTED_EDGE ( 'NONE', *, *, #4626, .T. ) ;
#728 = VECTOR ( 'NONE', #13325, 1000.000000000000000 ) ;
#729 = ORIENTED_EDGE ( 'NONE', *, *, #5793, .F. ) ;
#730 = VECTOR ( 'NONE', #11828, 1000.000000000000000 ) ;
#731 = VECTOR ( 'NONE', #11588, 1000.000000000000000 ) ;
#732 = VERTEX_POINT ( 'NONE', #2758 ) ;
#733 = ORIENTED_EDGE ( 'NONE', *, *, #13367, .T. ) ;
#734 = DIRECTION ( 'NONE',  ( -0.000000000000000000, -1.000000000000000000, -0.000000000000000000 ) ) ;
#735 = SURFACE_STYLE_USAGE ( .BOTH. , #2933 ) ;
#736 = EDGE_CURVE ( 'NONE', #7676, #11515, #12131, .T. ) ;
#737 = EDGE_CURVE ( 'NONE', #3503, #12047, #9277, .T. ) ;
#738 = CIRCLE ( 'NONE', #1389, 12.08999999999737440 ) ;
#739 = CARTESIAN_POINT ( 'NONE',  ( 53.04054522416362261, 3.000000000000000000, -3.611077387296437013 ) ) ;
#740 = AXIS2_PLACEMENT_3D ( 'NONE', #5209, #10447, #871 ) ;
#741 = PRESENTATION_LAYER_ASSIGNMENT (  '', '', ( #5350 ) ) ;
#742 = LINE ( 'NONE', #10031, #3726 ) ;
#743 = CARTESIAN_POINT ( 'NONE',  ( 7.771282357155270937, 9.000000000000000000, -3.443424244174282833 ) ) ;
#744 = CARTESIAN_POINT ( 'NONE',  ( -13.50994833511691340, 0.000000000000000000, -1.105736515254444052 ) ) ;
#745 = DIRECTION ( 'NONE',  ( 0.000000000000000000, 0.000000000000000000, 1.000000000000000000 ) ) ;
#746 = VERTEX_POINT ( 'NONE', #7028 ) ;
#747 = ORIENTED_EDGE ( 'NONE', *, *, #4870, .F. ) ;
#748 = VERTEX_POINT ( 'NONE', #8122 ) ;
#749 = AXIS2_PLACEMENT_3D ( 'NONE', #1426, #5473, #4586 ) ;
#750 = CARTESIAN_POINT ( 'NONE',  ( -13.04554897075795949, 3.000000000000000000, 5.733772933379550629 ) ) ;
#751 = CIRCLE ( 'NONE', #6016, 12.08999999999737440 ) ;
#752 = AXIS2_PLACEMENT_3D ( 'NONE', #5759, #540, #3011 ) ;
#753 = EDGE_CURVE ( 'NONE', #11680, #11839, #5026, .T. ) ;
#754 = ORIENTED_EDGE ( 'NONE', *, *, #11345, .T. ) ;
#755 = CARTESIAN_POINT ( 'NONE',  ( 11.11702303352194043, 0.000000000000000000, -8.914835885878249044 ) ) ;
#756 = CARTESIAN_POINT ( 'NONE',  ( 59.20906036370015357, 41.33135765298363395, 9.098535593488138673 ) ) ;
#757 = CARTESIAN_POINT ( 'NONE',  ( -11.70905276178463872, 3.000000000000000000, -9.375397774054366806 ) ) ;
#758 = DIRECTION ( 'NONE',  ( -0.000000000000000000, -1.000000000000000000, -0.000000000000000000 ) ) ;
#759 = CIRCLE ( 'NONE', #12438, 6.749999999999999112 ) ;
#760 = CARTESIAN_POINT ( 'NONE',  ( -8.922136023539609440, 3.000000000000000000, 8.158651161643900807 ) ) ;
#761 = CIRCLE ( 'NONE', #2511, 1.500000000000000222 ) ;
#762 = CYLINDRICAL_SURFACE ( 'NONE', #11276, 8.500000000000001776 ) ;
#763 = DIRECTION ( 'NONE',  ( 0.000000000000000000, 1.000000000000000000, 0.000000000000000000 ) ) ;
#764 = VECTOR ( 'NONE', #12228, 1000.000000000000000 ) ;
#765 = ORIENTED_EDGE ( 'NONE', *, *, #1720, .F. ) ;
#766 = CARTESIAN_POINT ( 'NONE',  ( 5.051606143860418285, 9.000000000000000000, 4.477027514692275112 ) ) ;
#767 = EDGE_LOOP ( 'NONE', ( #4537, #1649, #2280, #9539 ) ) ;
#768 = ORIENTED_EDGE ( 'NONE', *, *, #11051, .T. ) ;
#769 = FACE_OUTER_BOUND ( 'NONE', #7814, .T. ) ;
#770 = EDGE_CURVE ( 'NONE', #5898, #6650, #5857, .T. ) ;
#771 = EDGE_LOOP ( 'NONE', ( #11809, #6157, #8797, #4003 ) ) ;
#772 = AXIS2_PLACEMENT_3D ( 'NONE', #3729, #8758, #5667 ) ;
#773 = AXIS2_PLACEMENT_3D ( 'NONE', #5480, #10594, #1085 ) ;
#774 = ORIENTED_EDGE ( 'NONE', *, *, #4675, .F. ) ;
#775 = DIRECTION ( 'NONE',  ( -0.000000000000000000, -1.000000000000000000, -0.000000000000000000 ) ) ;
#776 = CARTESIAN_POINT ( 'NONE',  ( -13.52637830886139092, 3.000000000000000000, 2.928250210355532790 ) ) ;
#777 =( NAMED_UNIT ( * ) SI_UNIT ( $, .STERADIAN. ) SOLID_ANGLE_UNIT ( ) );
#778 = CARTESIAN_POINT ( 'NONE',  ( -7.668956737359326148, 9.000000000000000000, -2.066866683227997825 ) ) ;
#779 = CARTESIAN_POINT ( 'NONE',  ( -13.49999999999999645, 0.000000000000000000, -7.049999999999998934 ) ) ;
#780 = CARTESIAN_POINT ( 'NONE',  ( 0.000000000000000000, 0.000000000000000000, 0.000000000000000000 ) ) ;
#781 = VERTEX_POINT ( 'NONE', #627 ) ;
#782 = CIRCLE ( 'NONE', #5181, 1.500000000000000666 ) ;
#783 = CARTESIAN_POINT ( 'NONE',  ( -14.16466328168009881, 3.000000000000000000, 1.557181465540760534 ) ) ;
#784 = VECTOR ( 'NONE', #13170, 1000.000000000000000 ) ;
#785 = ORIENTED_EDGE ( 'NONE', *, *, #3659, .F. ) ;
#786 = EDGE_LOOP ( 'NONE', ( #2481, #7986, #11590, #10506 ) ) ;
#787 = CARTESIAN_POINT ( 'NONE',  ( 0.000000000000000000, 3.000000000000000000, 0.000000000000000000 ) ) ;
#788 = EDGE_CURVE ( 'NONE', #1247, #10439, #582, .T. ) ;
#789 = ORIENTED_EDGE ( 'NONE', *, *, #10527, .F. ) ;
#790 = CARTESIAN_POINT ( 'NONE',  ( 0.000000000000000000, 2.900000000000000355, 3.400000000000001243 ) ) ;
#791 = MECHANICAL_DESIGN_GEOMETRIC_PRESENTATION_REPRESENTATION (  '', ( #6937 ), #11784 ) ;
#792 = EDGE_CURVE ( 'NONE', #11192, #8134, #10615, .T. ) ;
#793 = VECTOR ( 'NONE', #337, 1000.000000000000000 ) ;
#794 = CARTESIAN_POINT ( 'NONE',  ( 20.03271148078819408, 0.000000000000000000, -5.075121771833452478 ) ) ;
#795 = EDGE_CURVE ( 'NONE', #291, #13143, #3919, .T. ) ;
#796 = CARTESIAN_POINT ( 'NONE',  ( -12.56087513340552242, 0.000000000000000000, 2.568302020731519253 ) ) ;
#797 = DIRECTION ( 'NONE',  ( 0.000000000000000000, 0.000000000000000000, 1.000000000000000000 ) ) ;
#798 = CARTESIAN_POINT ( 'NONE',  ( -13.50845331674225847, 3.000000000000000000, 1.119409668803372115 ) ) ;
#799 = CARTESIAN_POINT ( 'NONE',  ( 48.80418793193314997, 0.000000000000000000, -4.004112872419501201 ) ) ;
#800 = CARTESIAN_POINT ( 'NONE',  ( -6.506620931068715308, 3.000000000000000000, -10.18979803820051799 ) ) ;
#801 = CARTESIAN_POINT ( 'NONE',  ( 10.97318381393774089, 3.000000000000000000, -6.970598036433387712 ) ) ;
#802 = DIRECTION ( 'NONE',  ( -0.000000000000000000, -1.000000000000000000, -0.000000000000000000 ) ) ;
#803 = LINE ( 'NONE', #12094, #13042 ) ;
#804 = ORIENTED_EDGE ( 'NONE', *, *, #12412, .F. ) ;
#805 = AXIS2_PLACEMENT_3D ( 'NONE', #8112, #2667, #13145 ) ;
#806 = ORIENTED_EDGE ( 'NONE', *, *, #6747, .T. ) ;
#807 = ORIENTED_EDGE ( 'NONE', *, *, #13420, .F. ) ;
#808 = ORIENTED_EDGE ( 'NONE', *, *, #12116, .F. ) ;
#809 = CARTESIAN_POINT ( 'NONE',  ( 30.73000000000000043, 0.000000000000000000, -3.999999999999999112 ) ) ;
#810 = LINE ( 'NONE', #12316, #2307 ) ;
#811 = LINE ( 'NONE', #5002, #9521 ) ;
#812 = CARTESIAN_POINT ( 'NONE',  ( 7.500000000000003553, 3.000000000000000000, 4.899999999999997691 ) ) ;
#813 = CARTESIAN_POINT ( 'NONE',  ( 5.806472362263156661, -1.694065894508600678E-18, -5.419014975255640465 ) ) ;
#814 = DIRECTION ( 'NONE',  ( -0.4145344181384821858, 0.000000000000000000, 0.9100336346413741007 ) ) ;
#815 = CARTESIAN_POINT ( 'NONE',  ( 0.000000000000000000, 3.000000000000000000, 0.000000000000000000 ) ) ;
#816 = VERTEX_POINT ( 'NONE', #4965 ) ;
#817 = CARTESIAN_POINT ( 'NONE',  ( -10.69794375946289655, 3.000000000000000000, -7.065816209474156118 ) ) ;
#818 = CARTESIAN_POINT ( 'NONE',  ( 0.000000000000000000, 3.000000000000000000, -12.08999999999737440 ) ) ;
#819 = ORIENTED_EDGE ( 'NONE', *, *, #11292, .T. ) ;
#820 = B_SPLINE_CURVE_WITH_KNOTS ( 'NONE', 3,
 ( #13008, #12943, #6736, #7833 ),
 .UNSPECIFIED., .F., .F.,
 ( 4, 4 ),
 ( 0.1547128134717859205, 1.000000000000000000 ),
 .UNSPECIFIED. ) ;
#821 = FACE_OUTER_BOUND ( 'NONE', #2364, .T. ) ;
#822 = DIRECTION ( 'NONE',  ( -0.7094186368442984003, -1.178517763159896429E-26, -0.7047873421805881389 ) ) ;
#823 = CARTESIAN_POINT ( 'NONE',  ( 0.7702044561450380744, 0.000000000000000000, -12.79759916868914615 ) ) ;
#824 = DIRECTION ( 'NONE',  ( 0.000000000000000000, 0.000000000000000000, 1.000000000000000000 ) ) ;
#825 = CARTESIAN_POINT ( 'NONE',  ( 5.731782959214990036, 0.000000000000000000, 11.46814821560793618 ) ) ;
#826 = LINE ( 'NONE', #5339, #12157 ) ;
#827 = CARTESIAN_POINT ( 'NONE',  ( -12.51336114795298471, 3.000000000000000000, -3.542894103880322998 ) ) ;
#828 = ORIENTED_EDGE ( 'NONE', *, *, #11819, .T. ) ;
#829 = CARTESIAN_POINT ( 'NONE',  ( -12.76342233970728124, 3.000000000000000000, -4.564691384634500970 ) ) ;
#830 = ORIENTED_EDGE ( 'NONE', *, *, #11288, .T. ) ;
#831 = ORIENTED_EDGE ( 'NONE', *, *, #531, .F. ) ;
#832 = DIRECTION ( 'NONE',  ( 0.000000000000000000, 1.000000000000000000, -0.000000000000000000 ) ) ;
#833 = VERTEX_POINT ( 'NONE', #12065 ) ;
#834 = DIRECTION ( 'NONE',  ( 0.000000000000000000, 1.000000000000000000, -0.000000000000000000 ) ) ;
#835 =( LENGTH_UNIT ( ) NAMED_UNIT ( * ) SI_UNIT ( .MILLI., .METRE. ) );
#837 = FACE_OUTER_BOUND ( 'NONE', #2927, .T. ) ;
#836 = B_SPLINE_CURVE_WITH_KNOTS ( 'NONE', 2,
 ( #3497, #5499, #8595 ),
 .UNSPECIFIED., .F., .F.,
 ( 3, 3 ),
 ( 0.000000000000000000, 1.000000000000000000 ),
 .UNSPECIFIED. ) ;
#838 = DIRECTION ( 'NONE',  ( -0.000000000000000000, -1.000000000000000000, -0.000000000000000000 ) ) ;
#839 = DIRECTION ( 'NONE',  ( 0.000000000000000000, 0.000000000000000000, -1.000000000000000000 ) ) ;
#840 = CARTESIAN_POINT ( 'NONE',  ( 8.252687871541644071, 3.000000000000000000, 28.00000000000000000 ) ) ;
#841 = CARTESIAN_POINT ( 'NONE',  ( -13.04554897075799680, 3.000000000000000000, -5.733772933379471581 ) ) ;
#842 = EDGE_CURVE ( 'NONE', #5225, #11316, #7958, .T. ) ;
#843 = VERTEX_POINT ( 'NONE', #3647 ) ;
#844 = PRODUCT_RELATED_PRODUCT_CATEGORY ( 'part', '', ( #8958 ) ) ;
#845 = CARTESIAN_POINT ( 'NONE',  ( 3.061616997868383141E-16, 14.00000000000000178, 2.500000000000000000 ) ) ;
#846 = VERTEX_POINT ( 'NONE', #2681 ) ;
#847 = ORIENTED_EDGE ( 'NONE', *, *, #2780, .F. ) ;
#848 = CARTESIAN_POINT ( 'NONE',  ( 10.00000000000001421, 6.000000000000007105, -2.602085213965208275E-15 ) ) ;
#849 = ORIENTED_EDGE ( 'NONE', *, *, #6154, .F. ) ;
#850 = CARTESIAN_POINT ( 'NONE',  ( 0.000000000000000000, 2.900000000000000355, -1.500000000000000222 ) ) ;
#851 = PLANE ( 'NONE',  #4516 ) ;
#852 = CARTESIAN_POINT ( 'NONE',  ( 8.208497377870827449, 3.000000000000000000, -8.550000000000002487 ) ) ;
#853 = CARTESIAN_POINT ( 'NONE',  ( -5.999999999999991118, 0.000000000000000000, 28.50000000000000000 ) ) ;
#854 = DIRECTION ( 'NONE',  ( -1.000000000000000000, 0.000000000000000000, -0.000000000000000000 ) ) ;
#855 = CONTEXT_DEPENDENT_SHAPE_REPRESENTATION ( #11982, #10968 ) ;
#856 = CARTESIAN_POINT ( 'NONE',  ( 4.286263797015737088E-16, 3.000000000000000000, 3.500000000000000888 ) ) ;
#857 = EDGE_CURVE ( 'NONE', #12351, #4567, #10437, .T. ) ;
#858 = CARTESIAN_POINT ( 'NONE',  ( 6.025412986832064277, 0.000000000000000000, -13.73660796332615597 ) ) ;
#859 = DIRECTION ( 'NONE',  ( -0.000000000000000000, -1.000000000000000000, -0.000000000000000000 ) ) ;
#860 = EDGE_CURVE ( 'NONE', #10776, #641, #1589, .T. ) ;
#861 = ORIENTED_EDGE ( 'NONE', *, *, #8629, .F. ) ;
#862 = DIRECTION ( 'NONE',  ( -0.000000000000000000, -1.000000000000000000, -0.000000000000000000 ) ) ;
#863 = ORIENTED_EDGE ( 'NONE', *, *, #8463, .T. ) ;
#864 = EDGE_CURVE ( 'NONE', #8802, #6054, #283, .T. ) ;
#865 = ORIENTED_EDGE ( 'NONE', *, *, #444, .T. ) ;
#866 = EDGE_CURVE ( 'NONE', #10985, #3576, #2838, .T. ) ;
#867 = ORIENTED_EDGE ( 'NONE', *, *, #6355, .F. ) ;
#868 = VERTEX_POINT ( 'NONE', #2820 ) ;
#869 = DIRECTION ( 'NONE',  ( 0.000000000000000000, 0.000000000000000000, 1.000000000000000000 ) ) ;
#870 = CARTESIAN_POINT ( 'NONE',  ( 7.702138240596505092, 3.000000000000000000, -30.99999999999999289 ) ) ;
#871 = DIRECTION ( 'NONE',  ( 0.000000000000000000, 0.000000000000000000, 1.000000000000000000 ) ) ;
#872 = EDGE_CURVE ( 'NONE', #8783, #8207, #563, .T. ) ;
#873 = DIRECTION ( 'NONE',  ( -0.000000000000000000, -1.000000000000000000, -0.000000000000000000 ) ) ;
#874 = CARTESIAN_POINT ( 'NONE',  ( 7.712570079660896916, 3.000000000000000000, -11.14709020439929432 ) ) ;
#875 = DIRECTION ( 'NONE',  ( -0.000000000000000000, -1.000000000000000000, -0.000000000000000000 ) ) ;
#876 = CARTESIAN_POINT ( 'NONE',  ( 29.02231267299996986, 3.000000000000000000, -1.321950885510182250 ) ) ;
#877 = ORIENTED_EDGE ( 'NONE', *, *, #6306, .T. ) ;
#878 = ADVANCED_FACE ( 'NONE', ( #769 ), #579, .F. ) ;
#879 = LINE ( 'NONE', #11884, #4882 ) ;
#880 = CARTESIAN_POINT ( 'NONE',  ( 13.04554897075799502, 3.000000000000000000, 5.733772933379473358 ) ) ;
#881 = ORIENTED_EDGE ( 'NONE', *, *, #4007, .F. ) ;
#882 = CIRCLE ( 'NONE', #16, 3.399999999999999911 ) ;
#883 = DIRECTION ( 'NONE',  ( 0.000000000000000000, 1.000000000000000000, 0.000000000000000000 ) ) ;
#884 = PRODUCT_CONTEXT ( 'NONE', #2816, 'mechanical' ) ;
#885 = EDGE_CURVE ( 'NONE', #12346, #7762, #8457, .T. ) ;
#886 = CARTESIAN_POINT ( 'NONE',  ( 5.571433138827823761, 3.000000000000000000, 10.72973591378220704 ) ) ;
#887 = CARTESIAN_POINT ( 'NONE',  ( -11.48836750521723893, 3.000000000000000000, 8.430890348300625448 ) ) ;
#888 = EDGE_CURVE ( 'NONE', #7605, #5310, #5227, .T. ) ;
#889 = CARTESIAN_POINT ( 'NONE',  ( -7.798201703419567643, 3.000000000000000000, -27.99999999999999289 ) ) ;
#890 = CARTESIAN_POINT ( 'NONE',  ( 31.00000000000000000, 2.900000000000000355, 0.000000000000000000 ) ) ;
#891 = DIRECTION ( 'NONE',  ( -0.000000000000000000, -1.000000000000000000, -0.000000000000000000 ) ) ;
#892 = VECTOR ( 'NONE', #7735, 1000.000000000000000 ) ;
#893 = ORIENTED_EDGE ( 'NONE', *, *, #8265, .T. ) ;
#894 = VECTOR ( 'NONE', #3788, 1000.000000000000000 ) ;
#895 = B_SPLINE_CURVE_WITH_KNOTS ( 'NONE', 3,
 ( #4835, #5874, #2772, #9106 ),
 .UNSPECIFIED., .F., .F.,
 ( 4, 4 ),
 ( 0.1276832474596280298, 1.000000000000000000 ),
 .UNSPECIFIED. ) ;
#896 = UNCERTAINTY_MEASURE_WITH_UNIT (LENGTH_MEASURE( 1.000000000000000082E-05 ), #12069, 'distance_accuracy_value', 'NONE');
#897 = ORIENTED_EDGE ( 'NONE', *, *, #5905, .F. ) ;
#898 = DIRECTION ( 'NONE',  ( 0.7216024245882196597, 0.000000000000000000, 0.6923076923076926237 ) ) ;
#899 = VERTEX_POINT ( 'NONE', #2965 ) ;
#900 = CARTESIAN_POINT ( 'NONE',  ( 2.392396671352951198, 0.000000000000000000, 6.311809420990095454 ) ) ;
#901 = SURFACE_SIDE_STYLE ('',( #11166 ) ) ;
#902 = VECTOR ( 'NONE', #7758, 1000.000000000000000 ) ;
#903 = CARTESIAN_POINT ( 'NONE',  ( 0.000000000000000000, 0.09999999999999982514, 0.000000000000000000 ) ) ;
#904 = CARTESIAN_POINT ( 'NONE',  ( -2.375523406013125616, 9.000000000000000000, 6.318179211409232998 ) ) ;
#905 = AXIS2_PLACEMENT_3D ( 'NONE', #8919, #11968, #4655 ) ;
#906 = DIRECTION ( 'NONE',  ( 0.000000000000000000, 1.000000000000000000, 0.000000000000000000 ) ) ;
#907 = DIRECTION ( 'NONE',  ( 0.000000000000000000, 0.000000000000000000, 1.000000000000000000 ) ) ;
#908 = CARTESIAN_POINT ( 'NONE',  ( -13.97385902380755240, 0.000000000000000000, -5.452638258930474713 ) ) ;
#909 = EDGE_LOOP ( 'NONE', ( #5022, #6085, #12147, #4456 ) ) ;
#910 = CARTESIAN_POINT ( 'NONE',  ( 2.394769219159762041, 9.000000000000000000, -6.310909632292713844 ) ) ;
#911 = VERTEX_POINT ( 'NONE', #7174 ) ;
#912 = VERTEX_POINT ( 'NONE', #8318 ) ;
#913 = CARTESIAN_POINT ( 'NONE',  ( -4.821006024661084410, 3.000000000000000000, -13.61374091949017640 ) ) ;
#914 = AXIS2_PLACEMENT_3D ( 'NONE', #6046, #5067, #11412 ) ;
#915 = AXIS2_PLACEMENT_3D ( 'NONE', #514, #12237, #8971 ) ;
#916 = VERTEX_POINT ( 'NONE', #13435 ) ;
#917 = ADVANCED_FACE ( 'NONE', ( #5 ), #1999, .T. ) ;
#918 = CARTESIAN_POINT ( 'NONE',  ( -1.161309641800940540, 9.000000000000000000, -7.856984441350959969 ) ) ;
#919 = CARTESIAN_POINT ( 'NONE',  ( -6.721397655168936502, 0.000000000000000000, 5.203154193476255074 ) ) ;
#920 = CARTESIAN_POINT ( 'NONE',  ( 2.394769219159762930, 0.000000000000000000, -6.310909632292713844 ) ) ;
#921 = CARTESIAN_POINT ( 'NONE',  ( 31.00000000000000000, 3.000000000000000000, -1.073670993220974656E-09 ) ) ;
#922 = CARTESIAN_POINT ( 'NONE',  ( 48.80418793193314997, 3.000000000000000000, -4.004112872419501201 ) ) ;
#923 = CYLINDRICAL_SURFACE ( 'NONE', #4474, 1.499999999999997780 ) ;
#924 = VECTOR ( 'NONE', #7658, 1000.000000000000000 ) ;
#925 = FACE_OUTER_BOUND ( 'NONE', #3987, .T. ) ;
#926 = DIRECTION ( 'NONE',  ( 0.000000000000000000, 0.000000000000000000, -1.000000000000000000 ) ) ;
#927 = CARTESIAN_POINT ( 'NONE',  ( -2.568302020731516588, 0.000000000000000000, -12.56087513340552242 ) ) ;
#928 = EDGE_LOOP ( 'NONE', ( #5189, #8417, #11342, #4818 ) ) ;
#929 = CARTESIAN_POINT ( 'NONE',  ( -7.751044794789887504, 9.000000000000000000, 1.733822342365972879 ) ) ;
#930 = VERTEX_POINT ( 'NONE', #3159 ) ;
#931 = B_SPLINE_CURVE_WITH_KNOTS ( 'NONE', 3,
 ( #11785, #6404, #10616, #7446 ),
 .UNSPECIFIED., .F., .F.,
 ( 4, 4 ),
 ( 0.000000000000000000, 0.8452273900860258760 ),
 .UNSPECIFIED. ) ;
#932 = ORIENTED_EDGE ( 'NONE', *, *, #8564, .T. ) ;
#933 = VERTEX_POINT ( 'NONE', #4262 ) ;
#934 = CIRCLE ( 'NONE', #10828, 6.750000000000000888 ) ;
#935 = EDGE_CURVE ( 'NONE', #2130, #9763, #2355, .T. ) ;
#936 = EDGE_CURVE ( 'NONE', #7585, #7204, #7318, .T. ) ;
#937 = VERTEX_POINT ( 'NONE', #12487 ) ;
#938 = CARTESIAN_POINT ( 'NONE',  ( -11.90284147956865723, 0.000000000000000000, -9.133371500908332052 ) ) ;
#939 = CYLINDRICAL_SURFACE ( 'NONE', #12631, 14.25000000000000178 ) ;
#940 = LINE ( 'NONE', #9342, #5056 ) ;
#941 = DIRECTION ( 'NONE',  ( 0.000000000000000000, 0.000000000000000000, 1.000000000000000000 ) ) ;
#942 = VECTOR ( 'NONE', #5646, 1000.000000000000000 ) ;
#943 = AXIS2_PLACEMENT_3D ( 'NONE', #4491, #8681, #11656 ) ;
#944 = LINE ( 'NONE', #5143, #12861 ) ;
#945 = DIRECTION ( 'NONE',  ( 0.000000000000000000, 1.000000000000000000, -0.000000000000000000 ) ) ;
#946 = EDGE_LOOP ( 'NONE', ( #12130, #12248, #7141, #189 ) ) ;
#947 = ORIENTED_EDGE ( 'NONE', *, *, #12559, .T. ) ;
#948 = CARTESIAN_POINT ( 'NONE',  ( 11.46847481510586775, 3.000000000000000000, 5.708888906988908829 ) ) ;
#949 = EDGE_CURVE ( 'NONE', #11231, #5642, #6128, .T. ) ;
#950 = ORIENTED_EDGE ( 'NONE', *, *, #13438, .T. ) ;
#951 = CARTESIAN_POINT ( 'NONE',  ( 8.482622935103764306, 0.000000000000000000, -9.600126836553261711 ) ) ;
#952 = AXIS2_PLACEMENT_3D ( 'NONE', #7370, #1092, #8383 ) ;
#953 = VECTOR ( 'NONE', #5138, 1000.000000000000000 ) ;
#954 = DIRECTION ( 'NONE',  ( 0.000000000000000000, 0.000000000000000000, 1.000000000000000000 ) ) ;
#955 = EDGE_CURVE ( 'NONE', #10261, #8040, #6326, .T. ) ;
#956 = PRODUCT_CONTEXT ( 'NONE', #1418, 'mechanical' ) ;
#957 = ADVANCED_FACE ( 'NONE', ( #78 ), #10534, .T. ) ;
#958 = CARTESIAN_POINT ( 'NONE',  ( 0.5398653231797245766, 0.000000000000000000, -12.07794044664754018 ) ) ;
#959 = CARTESIAN_POINT ( 'NONE',  ( 12.48034623170854474, 3.000000000000000000, 4.337627373772809491 ) ) ;
#960 = CARTESIAN_POINT ( 'NONE',  ( 0.000000000000000000, 9.000000000000000000, 0.000000000000000000 ) ) ;
#961 = DIRECTION ( 'NONE',  ( -0.000000000000000000, -1.000000000000000000, -0.000000000000000000 ) ) ;
#962 = AXIS2_PLACEMENT_3D ( 'NONE', #3139, #7989, #12209 ) ;
#963 = CARTESIAN_POINT ( 'NONE',  ( 12.03251085770905959, 0.000000000000000000, 3.999999998926332179 ) ) ;
#964 = VECTOR ( 'NONE', #3111, 1000.000000000000000 ) ;
#965 = CIRCLE ( 'NONE', #752, 0.4000000000000000222 ) ;
#966 = ORIENTED_EDGE ( 'NONE', *, *, #7209, .T. ) ;
#967 = ORIENTED_EDGE ( 'NONE', *, *, #13406, .T. ) ;
#968 = DIRECTION ( 'NONE',  ( -0.000000000000000000, -1.000000000000000000, 0.000000000000000000 ) ) ;
#969 = EDGE_CURVE ( 'NONE', #12363, #7708, #11509, .T. ) ;
#970 = ORIENTED_EDGE ( 'NONE', *, *, #8931, .T. ) ;
#971 = DIRECTION ( 'NONE',  ( 0.000000000000000000, 0.000000000000000000, 1.000000000000000000 ) ) ;
#972 = VECTOR ( 'NONE', #2138, 1000.000000000000000 ) ;
#973 = CARTESIAN_POINT ( 'NONE',  ( -14.82803603298498629, 0.000000000000000000, 2.264806262023049577 ) ) ;
#974 = CARTESIAN_POINT ( 'NONE',  ( 11.59535436762926430, 3.000000000000000000, -5.877734009726468756 ) ) ;
#975 = CARTESIAN_POINT ( 'NONE',  ( 3.469446951953614189E-15, 0.000000000000000000, -20.55000000000000071 ) ) ;
#976 = CARTESIAN_POINT ( 'NONE',  ( 31.00000000000000000, 2.900000000000000355, 0.000000000000000000 ) ) ;
#977 = DIRECTION ( 'NONE',  ( 0.7772490812545771455, 0.000000000000000000, 0.6291930273683233876 ) ) ;
#978 = ORIENTED_EDGE ( 'NONE', *, *, #10739, .T. ) ;
#979 = CARTESIAN_POINT ( 'NONE',  ( -5.571433138827826426, 3.000000000000000000, -10.72973591378220526 ) ) ;
#980 = ORIENTED_EDGE ( 'NONE', *, *, #10718, .T. ) ;
#981 = AXIS2_PLACEMENT_3D ( 'NONE', #7760, #6861, #5625 ) ;
#982 = ORIENTED_EDGE ( 'NONE', *, *, #13564, .F. ) ;
#983 = AXIS2_PLACEMENT_3D ( 'NONE', #6603, #5774, #12198 ) ;
#984 = CARTESIAN_POINT ( 'NONE',  ( 2.601737331980797041, 9.000000000000000000, -6.888123234756056590 ) ) ;
#985 = B_SPLINE_CURVE_WITH_KNOTS ( 'NONE', 3,
 ( #4368, #8556, #9667, #12778 ),
 .UNSPECIFIED., .F., .F.,
 ( 4, 4 ),
 ( 0.000000000000000000, 0.8452273900860258760 ),
 .UNSPECIFIED. ) ;
#986 = EDGE_CURVE ( 'NONE', #1347, #525, #738, .T. ) ;
#987 = EDGE_CURVE ( 'NONE', #13268, #8754, #11578, .T. ) ;
#988 = ORIENTED_EDGE ( 'NONE', *, *, #11808, .T. ) ;
#989 = CARTESIAN_POINT ( 'NONE',  ( 0.000000000000000000, 9.000000000000000000, 0.000000000000000000 ) ) ;
#990 = CARTESIAN_POINT ( 'NONE',  ( 11.59535436762926430, 3.000000000000000000, -5.877734009726468756 ) ) ;
#991 = LINE ( 'NONE', #852, #68 ) ;
#992 = CYLINDRICAL_SURFACE ( 'NONE', #3950, 2.500000000000000000 ) ;
#993 = B_SPLINE_CURVE_WITH_KNOTS ( 'NONE', 3,
 ( #11149, #12478, #3016, #10103 ),
 .UNSPECIFIED., .F., .F.,
 ( 4, 4 ),
 ( 0.1547128134717859205, 1.000000000000000000 ),
 .UNSPECIFIED. ) ;
#994 = CARTESIAN_POINT ( 'NONE',  ( 12.00000000000000533, 2.749999999999991118, 10.00000000000000000 ) ) ;
#995 = ITEM_DEFINED_TRANSFORMATION ( 'NONE', 'NONE', #10480,  #10007 ) ;
#996 = CIRCLE ( 'NONE', #4722, 1.500000000000001332 ) ;
#997 = LINE ( 'NONE', #13463, #7125 ) ;
#998 = VECTOR ( 'NONE', #2423, 1000.000000000000114 ) ;
#999 = FACE_OUTER_BOUND ( 'NONE', #9309, .T. ) ;
#1000 = CARTESIAN_POINT ( 'NONE',  ( 11.48836750521724070, 0.000000000000000000, 8.430890348300627224 ) ) ;
#1001 = ORIENTED_EDGE ( 'NONE', *, *, #5458, .F. ) ;
#1002 = LINE ( 'NONE', #11939, #11502 ) ;
#1003 = EDGE_LOOP ( 'NONE', ( #12475, #4348 ) ) ;
#1004 = VERTEX_POINT ( 'NONE', #8188 ) ;
#1005 = ORIENTED_EDGE ( 'NONE', *, *, #10913, .T. ) ;
#1006 = PRESENTATION_LAYER_ASSIGNMENT (  '', '', ( #6937 ) ) ;
#1007 = VECTOR ( 'NONE', #3151, 1000.000000000000000 ) ;
#1008 = VERTEX_POINT ( 'NONE', #7434 ) ;
#1009 = CARTESIAN_POINT ( 'NONE',  ( -8.914835885878282795, 3.000000000000000000, -11.11702303352191556 ) ) ;
#1010 = CARTESIAN_POINT ( 'NONE',  ( 31.00000000000000000, 0.09999999999999982514, 0.000000000000000000 ) ) ;
#1011 = DIRECTION ( 'NONE',  ( 0.000000000000000000, 0.000000000000000000, 1.000000000000000000 ) ) ;
#1012 = CARTESIAN_POINT ( 'NONE',  ( 30.65246752842885058, 3.000000000000000000, -7.988606140548566437 ) ) ;
#1013 = CARTESIAN_POINT ( 'NONE',  ( -7.712570079660889810, 3.000000000000000000, 11.14709020439930320 ) ) ;
#1014 = COLOUR_RGB ( '',0.7803921568627451011, 0.7607843137254901578, 0.7411764705882353255 ) ;
#1015 = EDGE_CURVE ( 'NONE', #1814, #11917, #3181, .T. ) ;
#1016 = ORIENTED_EDGE ( 'NONE', *, *, #5815, .F. ) ;
#1017 = CARTESIAN_POINT ( 'NONE',  ( -11.48836750521728689, 3.000000000000000000, -8.430890348300561499 ) ) ;
#1018 = DIRECTION ( 'NONE',  ( 0.000000000000000000, 0.000000000000000000, -1.000000000000000000 ) ) ;
#1019 = ORIENTED_EDGE ( 'NONE', *, *, #13582, .T. ) ;
#1020 = AXIS2_PLACEMENT_3D ( 'NONE', #1463, #1670, #8523 ) ;
#1021 = CARTESIAN_POINT ( 'NONE',  ( -11.48836750521728867, 3.000000000000000000, -8.430890348300557946 ) ) ;
#1022 = LINE ( 'NONE', #9481, #434 ) ;
#1023 = DIRECTION ( 'NONE',  ( 1.000000000000000000, 0.000000000000000000, 0.000000000000000000 ) ) ;
#1024 = FACE_BOUND ( 'NONE', #7694, .T. ) ;
#1025 = CARTESIAN_POINT ( 'NONE',  ( 10.98198414889934682, 3.000000000000000000, -9.379342464487748998 ) ) ;
#1026 = CARTESIAN_POINT ( 'NONE',  ( 28.47439151394123158, 2.900000000000000355, -2.423076923076924682 ) ) ;
#1027 = CARTESIAN_POINT ( 'NONE',  ( -11.52330688609014686, 0.000000000000000000, -6.017756925049552841 ) ) ;
#1028 = LINE ( 'NONE', #10468, #1408 ) ;
#1029 = EDGE_LOOP ( 'NONE', ( #6359, #8832, #10154, #3644 ) ) ;
#1030 = EDGE_CURVE ( 'NONE', #2354, #12940, #6015, .T. ) ;
#1031 = ORIENTED_EDGE ( 'NONE', *, *, #12543, .T. ) ;
#1032 = CARTESIAN_POINT ( 'NONE',  ( 0.1834774187694905023, 0.000000000000000000, -13.00394734430440025 ) ) ;
#1033 = EDGE_CURVE ( 'NONE', #6631, #1278, #9301, .T. ) ;
#1034 = ORIENTED_EDGE ( 'NONE', *, *, #10476, .T. ) ;
#1035 = DIRECTION ( 'NONE',  ( 0.000000000000000000, 0.000000000000000000, 1.000000000000000000 ) ) ;
#1036 = SURFACE_SIDE_STYLE ('',( #4266 ) ) ;
#1037 = DIRECTION ( 'NONE',  ( -0.7772490812545750360, 0.000000000000000000, -0.6291930273683260522 ) ) ;
#1038 = DIRECTION ( 'NONE',  ( -0.000000000000000000, 1.000000000000000000, -0.000000000000000000 ) ) ;
#1039 = CARTESIAN_POINT ( 'NONE',  ( -9.379342464487789854, 3.000000000000000000, -10.98198414889931307 ) ) ;
#1040 = B_SPLINE_CURVE_WITH_KNOTS ( 'NONE', 3,
 ( #2636, #10227, #3879, #8086 ),
 .UNSPECIFIED., .F., .F.,
 ( 4, 4 ),
 ( 0.000000000000000000, 0.5855695330273008592 ),
 .UNSPECIFIED. ) ;
#1041 = EDGE_CURVE ( 'NONE', #6903, #7175, #2191, .T. ) ;
#1042 = DIRECTION ( 'NONE',  ( 0.000000000000000000, 1.000000000000000000, -0.000000000000000000 ) ) ;
#1043 = DIRECTION ( 'NONE',  ( -0.000000000000000000, -1.000000000000000000, -0.000000000000000000 ) ) ;
#1044 = ORIENTED_EDGE ( 'NONE', *, *, #12723, .T. ) ;
#1045 = CARTESIAN_POINT ( 'NONE',  ( 0.000000000000000000, 0.000000000000000000, 0.000000000000000000 ) ) ;
#1046 = EDGE_LOOP ( 'NONE', ( #8671, #13240, #543, #1474 ) ) ;
#1047 = ORIENTED_EDGE ( 'NONE', *, *, #6279, .F. ) ;
#1048 = CARTESIAN_POINT ( 'NONE',  ( -5.741477348071430065, 3.000000000000000000, -13.86115248177175374 ) ) ;
#1049 = EDGE_CURVE ( 'NONE', #10250, #2353, #8420, .T. ) ;
#1050 = ORIENTED_EDGE ( 'NONE', *, *, #6088, .F. ) ;
#1051 = CARTESIAN_POINT ( 'NONE',  ( 1.133238802859644956, 3.000000000000000000, -14.39763212228013600 ) ) ;
#1052 = FACE_OUTER_BOUND ( 'NONE', #12922, .T. ) ;
#1053 = DIRECTION ( 'NONE',  ( -0.000000000000000000, -1.000000000000000000, -0.000000000000000000 ) ) ;
#1054 = CARTESIAN_POINT ( 'NONE',  ( 0.000000000000000000, 3.000000000000000000, 0.000000000000000000 ) ) ;
#1055 = DIRECTION ( 'NONE',  ( 0.000000000000000000, 0.000000000000000000, 1.000000000000000000 ) ) ;
#1056 = CARTESIAN_POINT ( 'NONE',  ( -6.524296280129988190, 0.000000000000000000, -3.413039245436654490 ) ) ;
#1057 = EDGE_CURVE ( 'NONE', #8876, #11924, #1835, .T. ) ;
#1058 = DIRECTION ( 'NONE',  ( 0.000000000000000000, 0.000000000000000000, -1.000000000000000000 ) ) ;
#1059 = EDGE_CURVE ( 'NONE', #2378, #12695, #10874, .T. ) ;
#1060 = DIRECTION ( 'NONE',  ( 0.000000000000000000, 0.000000000000000000, 1.000000000000000000 ) ) ;
#1061 = VERTEX_POINT ( 'NONE', #7768 ) ;
#1062 = FACE_OUTER_BOUND ( 'NONE', #6446, .T. ) ;
#1063 = VERTEX_POINT ( 'NONE', #2537 ) ;
#1064 = PRODUCT_DEFINITION_SHAPE ( 'NONE', 'NONE',  #13603 ) ;
#1065 = ORIENTED_EDGE ( 'NONE', *, *, #6952, .T. ) ;
#1066 = EDGE_CURVE ( 'NONE', #1278, #9479, #1841, .T. ) ;
#1067 = ORIENTED_EDGE ( 'NONE', *, *, #1799, .F. ) ;
#1068 = ORIENTED_EDGE ( 'NONE', *, *, #2402, .F. ) ;
#1069 = CARTESIAN_POINT ( 'NONE',  ( -13.82336506795071607, 3.000000000000000000, 0.6724118135763649251 ) ) ;
#1070 = CARTESIAN_POINT ( 'NONE',  ( 5.250000000000000000, 0.000000000000000000, -27.94078293894052578 ) ) ;
#1071 = DIRECTION ( 'NONE',  ( -2.312964634635743450E-15, -1.000000000000000000, 0.000000000000000000 ) ) ;
#1072 = CARTESIAN_POINT ( 'NONE',  ( 11.48836750521724070, 3.000000000000000000, 8.430890348300627224 ) ) ;
#1073 = CARTESIAN_POINT ( 'NONE',  ( -6.506507307819711095, 3.000000000000000000, 10.18987059060247624 ) ) ;
#1074 = DIRECTION ( 'NONE',  ( -0.000000000000000000, -1.000000000000000000, -0.000000000000000000 ) ) ;
#1075 = ORIENTED_EDGE ( 'NONE', *, *, #12735, .T. ) ;
#1076 = ORIENTED_EDGE ( 'NONE', *, *, #125, .T. ) ;
#1077 = DIRECTION ( 'NONE',  ( -0.000000000000000000, -1.000000000000000000, -0.000000000000000000 ) ) ;
#1078 = ORIENTED_EDGE ( 'NONE', *, *, #6023, .T. ) ;
#1079 = CARTESIAN_POINT ( 'NONE',  ( -3.833392836528144443, 9.000000000000000000, -5.555861711818853799 ) ) ;
#1080 = ADVANCED_FACE ( 'NONE', ( #4393 ), #6669, .T. ) ;
#1081 = CARTESIAN_POINT ( 'NONE',  ( 6.000000000000008882, 3.000000000000000000, 25.50000000000000000 ) ) ;
#1082 = APPLICATION_PROTOCOL_DEFINITION ( 'draft international standard', 'automotive_design', 1998, #12167 ) ;
#1083 = CARTESIAN_POINT ( 'NONE',  ( 8.180229652970799847, 3.000000000000000000, -11.90209577080762848 ) ) ;
#1084 = CARTESIAN_POINT ( 'NONE',  ( 31.00000000000000000, 0.09999999999999982514, 0.000000000000000000 ) ) ;
#1085 = DIRECTION ( 'NONE',  ( 0.000000000000000000, 0.000000000000000000, 1.000000000000000000 ) ) ;
#1086 = CARTESIAN_POINT ( 'NONE',  ( 3.061616997868383141E-16, 14.00000000000000178, 2.500000000000000000 ) ) ;
#1087 = DIRECTION ( 'NONE',  ( -1.000000000000000000, -0.000000000000000000, -0.000000000000000000 ) ) ;
#1088 = VERTEX_POINT ( 'NONE', #8584 ) ;
#1089 = B_SPLINE_CURVE_WITH_KNOTS ( 'NONE', 3,
 ( #12109, #4593, #4863, #1710 ),
 .UNSPECIFIED., .F., .F.,
 ( 4, 4 ),
 ( 0.000000000000000000, 0.8452273900860258760 ),
 .UNSPECIFIED. ) ;
#1090 = VERTEX_POINT ( 'NONE', #6467 ) ;
#1091 = VERTEX_POINT ( 'NONE', #9764 ) ;
#1092 = DIRECTION ( 'NONE',  ( 0.000000000000000000, 1.000000000000000000, -0.000000000000000000 ) ) ;
#1093 = AXIS2_PLACEMENT_3D ( 'NONE', #10679, #9375, #8321 ) ;
#1094 = ORIENTED_EDGE ( 'NONE', *, *, #10459, .T. ) ;
#1095 = EDGE_CURVE ( 'NONE', #1291, #11338, #12829, .T. ) ;
#1096 = ADVANCED_FACE ( 'NONE', ( #10676 ), #4245, .T. ) ;
#1097 = CARTESIAN_POINT ( 'NONE',  ( -6.934601996837493232, 9.000000000000000000, 3.871968458191308748 ) ) ;
#1098 =( NAMED_UNIT ( * ) SI_UNIT ( $, .STERADIAN. ) SOLID_ANGLE_UNIT ( ) );
#1099 = CARTESIAN_POINT ( 'NONE',  ( 6.329356821613516537, 0.000000000000000000, -12.30759122141987305 ) ) ;
#1100 = DIRECTION ( 'NONE',  ( 0.000000000000000000, 0.000000000000000000, 1.000000000000000000 ) ) ;
#1101 = CARTESIAN_POINT ( 'NONE',  ( -10.67828022838850721, 3.000000000000000000, 7.077546079049267469 ) ) ;
#1102 = EDGE_CURVE ( 'NONE', #43, #2399, #1440, .T. ) ;
#1103 = VECTOR ( 'NONE', #6151, 1000.000000000000000 ) ;
#1104 = CARTESIAN_POINT ( 'NONE',  ( -14.08504230442586369, 0.000000000000000000, 2.161962830978781724 ) ) ;
#1105 = AXIS2_PLACEMENT_3D ( 'NONE', #12702, #10697, #12762 ) ;
#1106 = FACE_OUTER_BOUND ( 'NONE', #909, .T. ) ;
#1107 = ORIENTED_EDGE ( 'NONE', *, *, #3844, .F. ) ;
#1108 = DIRECTION ( 'NONE',  ( 0.000000000000000000, 1.000000000000000000, 0.000000000000000000 ) ) ;
#1109 = ORIENTED_EDGE ( 'NONE', *, *, #8696, .F. ) ;
#1110 = VERTEX_POINT ( 'NONE', #5486 ) ;
#1111 = VERTEX_POINT ( 'NONE', #2338 ) ;
#1112 = CARTESIAN_POINT ( 'NONE',  ( -8.914835885878282795, 0.000000000000000000, -11.11702303352191556 ) ) ;
#1113 = ORIENTED_EDGE ( 'NONE', *, *, #9512, .F. ) ;
#1114 = AXIS2_PLACEMENT_3D ( 'NONE', #5964, #10032, #10093 ) ;
#1115 = EDGE_CURVE ( 'NONE', #3649, #2964, #8630, .T. ) ;
#1116 = CIRCLE ( 'NONE', #9239, 0.1000000000000001166 ) ;
#1117 = CARTESIAN_POINT ( 'NONE',  ( 30.66173999750687784, 0.000000000000000000, 0.01003121477750366919 ) ) ;
#1118 = DIRECTION ( 'NONE',  ( -0.000000000000000000, -1.000000000000000000, -0.000000000000000000 ) ) ;
#1119 = DIRECTION ( 'NONE',  ( 0.000000000000000000, 0.000000000000000000, 1.000000000000000000 ) ) ;
#1120 = DIRECTION ( 'NONE',  ( 0.000000000000000000, 1.000000000000000000, 0.000000000000000000 ) ) ;
#1121 = FACE_OUTER_BOUND ( 'NONE', #431, .T. ) ;
#1122 = EDGE_CURVE ( 'NONE', #4943, #748, #7568, .T. ) ;
#1123 = CARTESIAN_POINT ( 'NONE',  ( 3.818534268238711782, 0.000000000000000000, -5.566084444408534004 ) ) ;
#1124 = EDGE_CURVE ( 'NONE', #3555, #5490, #86, .T. ) ;
#1125 = FACE_OUTER_BOUND ( 'NONE', #10996, .T. ) ;
#1126 = CARTESIAN_POINT ( 'NONE',  ( 0.000000000000000000, 3.000000000000000000, -1.500000000000000222 ) ) ;
#1127 = ORIENTED_EDGE ( 'NONE', *, *, #9053, .T. ) ;
#1128 = CARTESIAN_POINT ( 'NONE',  ( 3.647599401157688437, 0.000000000000000000, 11.52662650599083882 ) ) ;
#1129 = AXIS2_PLACEMENT_3D ( 'NONE', #6919, #2580, #11188 ) ;
#1130 = CIRCLE ( 'NONE', #7717, 2.000000000000000444 ) ;
#1131 = ORIENTED_EDGE ( 'NONE', *, *, #11631, .F. ) ;
#1132 = EDGE_LOOP ( 'NONE', ( #13487, #412, #2430, #1761 ) ) ;
#1133 = EDGE_LOOP ( 'NONE', ( #9505, #3278, #13431, #10279 ) ) ;
#1134 = EDGE_CURVE ( 'NONE', #7270, #9350, #11725, .T. ) ;
#1135 = CARTESIAN_POINT ( 'NONE',  ( 4.369710415961185035, 0.000000000000000000, 6.632530905044255576 ) ) ;
#1136 = DIRECTION ( 'NONE',  ( 2.602085213965210149E-16, 0.000000000000000000, 1.000000000000000000 ) ) ;
#1137 = AXIS2_PLACEMENT_3D ( 'NONE', #10482, #6075, #10412 ) ;
#1138 = CARTESIAN_POINT ( 'NONE',  ( 11.70905276178455878, 3.000000000000000000, -9.375397774054460953 ) ) ;
#1139 = FACE_OUTER_BOUND ( 'NONE', #4650, .T. ) ;
#1140 = CARTESIAN_POINT ( 'NONE',  ( 30.73000000000000043, 0.000000000000000000, -5.500000000000003553 ) ) ;
#1141 = DIRECTION ( 'NONE',  ( 0.000000000000000000, 0.000000000000000000, 1.000000000000000000 ) ) ;
#1142 = VERTEX_POINT ( 'NONE', #10736 ) ;
#1143 = CIRCLE ( 'NONE', #10825, 0.09999999999999982514 ) ;
#1144 = ORIENTED_EDGE ( 'NONE', *, *, #7271, .F. ) ;
#1145 = CIRCLE ( 'NONE', #4886, 0.7500000000000024425 ) ;
#1146 = CARTESIAN_POINT ( 'NONE',  ( 3.000000000000001776, 2.000000000000000000, 10.00000000000000000 ) ) ;
#1147 = B_SPLINE_SURFACE_WITH_KNOTS ( 'NONE', 3, 1, ( 
 ( #8479, #9446 ),
 ( #12633, #11726 ),
 ( #8604, #11597 ),
 ( #6215, #2286 ) ),
 .UNSPECIFIED., .F., .F., .F.,
 ( 4, 4 ),
 ( 2, 2 ),
 ( 0.9090903094065657664, 0.9385083864668765097 ),
 ( 0.000000000000000000, 1.000000000000000000 ),
 .UNSPECIFIED. ) ;
#1148 = EDGE_CURVE ( 'NONE', #8355, #2851, #12877, .T. ) ;
#1149 = ORIENTED_EDGE ( 'NONE', *, *, #9004, .F. ) ;
#1150 = DIRECTION ( 'NONE',  ( 0.7772490812545826966, 0.000000000000000000, 0.6291930273683166153 ) ) ;
#1151 = DIRECTION ( 'NONE',  ( -0.000000000000000000, -1.000000000000000000, -0.000000000000000000 ) ) ;
#1152 = AXIS2_PLACEMENT_3D ( 'NONE', #10267, #11093, #13302 ) ;
#1153 = VECTOR ( 'NONE', #7917, 1000.000000000000000 ) ;
#1154 = DIRECTION ( 'NONE',  ( 0.000000000000000000, 1.000000000000000000, 0.000000000000000000 ) ) ;
#1155 = DIRECTION ( 'NONE',  ( 0.000000000000000000, 1.000000000000000000, -0.000000000000000000 ) ) ;
#1156 = CARTESIAN_POINT ( 'NONE',  ( -12.25836857253663759, 3.000000000000000000, -5.784789447945487773 ) ) ;
#1157 = DIRECTION ( 'NONE',  ( 0.000000000000000000, 1.000000000000000000, -0.000000000000000000 ) ) ;
#1158 = DIRECTION ( 'NONE',  ( -0.000000000000000000, -1.000000000000000000, -0.000000000000000000 ) ) ;
#1159 = VERTEX_POINT ( 'NONE', #4600 ) ;
#1160 = ORIENTED_EDGE ( 'NONE', *, *, #11475, .F. ) ;
#1161 = AXIS2_PLACEMENT_3D ( 'NONE', #2598, #10999, #1573 ) ;
#1162 = VERTEX_POINT ( 'NONE', #13006 ) ;
#1163 = CARTESIAN_POINT ( 'NONE',  ( -13.49999999999999645, 3.000000000000000000, -7.049999999999998934 ) ) ;
#1164 = AXIS2_PLACEMENT_3D ( 'NONE', #7954, #12178, #661 ) ;
#1165 = MECHANICAL_DESIGN_GEOMETRIC_PRESENTATION_REPRESENTATION (  '', ( #11512 ), #8633 ) ;
#1166 = ORIENTED_EDGE ( 'NONE', *, *, #5988, .F. ) ;
#1167 = FACE_BOUND ( 'NONE', #595, .T. ) ;
#1168 = PRESENTATION_STYLE_ASSIGNMENT (( #7377 ) ) ;
#1169 = FACE_OUTER_BOUND ( 'NONE', #1046, .T. ) ;
#1170 = B_SPLINE_CURVE_WITH_KNOTS ( 'NONE', 3,
 ( #10667, #12996, #2455, #1227 ),
 .UNSPECIFIED., .F., .F.,
 ( 4, 4 ),
 ( 0.1547128134717859205, 1.000000000000000000 ),
 .UNSPECIFIED. ) ;
#1171 = AXIS2_PLACEMENT_3D ( 'NONE', #3827, #4855, #8029 ) ;
#1172 = DIRECTION ( 'NONE',  ( 0.000000000000000000, 1.000000000000000000, -0.000000000000000000 ) ) ;
#1173 = CARTESIAN_POINT ( 'NONE',  ( -1.650143266773857142, 0.000000000000000000, -14.90895795148409952 ) ) ;
#1174 = CIRCLE ( 'NONE', #740, 1.499999999999999556 ) ;
#1175 = CIRCLE ( 'NONE', #6230, 14.25000000000000178 ) ;
#1176 = B_SPLINE_CURVE_WITH_KNOTS ( 'NONE', 3,
 ( #9855, #7659, #4562, #9597 ),
 .UNSPECIFIED., .F., .F.,
 ( 4, 4 ),
 ( 0.000000000000000000, 0.5855695330273008592 ),
 .UNSPECIFIED. ) ;
#1177 = CARTESIAN_POINT ( 'NONE',  ( -2.375523406013128280, 0.000000000000000000, 6.318179211409232998 ) ) ;
#1178 = DIRECTION ( 'NONE',  ( 0.000000000000000000, 0.000000000000000000, -1.000000000000000000 ) ) ;
#1179 = EDGE_LOOP ( 'NONE', ( #9943, #1067, #11868, #4169 ) ) ;
#1180 = DIRECTION ( 'NONE',  ( 0.000000000000000000, 0.000000000000000000, -1.000000000000000000 ) ) ;
#1181 = ORIENTED_EDGE ( 'NONE', *, *, #11088, .T. ) ;
#1182 = ORIENTED_EDGE ( 'NONE', *, *, #3026, .T. ) ;
#1183 = EDGE_CURVE ( 'NONE', #6311, #7408, #12402, .T. ) ;
#1184 = PRODUCT_RELATED_PRODUCT_CATEGORY ( 'part', '', ( #4340 ) ) ;
#1185 = ORIENTED_EDGE ( 'NONE', *, *, #10601, .F. ) ;
#1186 = CARTESIAN_POINT ( 'NONE',  ( 0.000000000000000000, 3.000000000000000000, 0.000000000000000000 ) ) ;
#1187 = ORIENTED_EDGE ( 'NONE', *, *, #8298, .F. ) ;
#1188 = AXIS2_PLACEMENT_3D ( 'NONE', #809, #5000, #9194 ) ;
#1189 = AXIS2_PLACEMENT_3D ( 'NONE', #12887, #3430, #7642 ) ;
#1190 = CARTESIAN_POINT ( 'NONE',  ( 9.299128225235451239, 3.000000000000000000, -10.25006213149493561 ) ) ;
#1191 = CARTESIAN_POINT ( 'NONE',  ( -5.999999999999991118, 3.000000000000000000, 27.00000000000000000 ) ) ;
#1192 = CARTESIAN_POINT ( 'NONE',  ( 0.000000000000000000, 0.000000000000000000, -0.4000000000000000222 ) ) ;
#1193 = CARTESIAN_POINT ( 'NONE',  ( -12.16218796965919324, 3.000000000000000000, -4.056222772158363021 ) ) ;
#1194 = LINE ( 'NONE', #10898, #1407 ) ;
#1195 = LINE ( 'NONE', #173, #5307 ) ;
#1196 = CARTESIAN_POINT ( 'NONE',  ( 11.14709020439929787, 0.000000000000000000, 7.712570079660892475 ) ) ;
#1197 = ORIENTED_EDGE ( 'NONE', *, *, #4427, .T. ) ;
#1198 = AXIS2_PLACEMENT_3D ( 'NONE', #5757, #8985, #538 ) ;
#1199 = DIRECTION ( 'NONE',  ( -0.5795187626277481518, -0.000000000000000000, -0.8149588969772669778 ) ) ;
#1200 = CIRCLE ( 'NONE', #4715, 2.500000000000000444 ) ;
#1201 = EDGE_CURVE ( 'NONE', #9963, #12046, #1703, .T. ) ;
#1202 = ORIENTED_EDGE ( 'NONE', *, *, #10865, .F. ) ;
#1203 = EDGE_CURVE ( 'NONE', #4274, #6311, #9519, .T. ) ;
#1204 = ORIENTED_EDGE ( 'NONE', *, *, #12712, .F. ) ;
#1205 = ORIENTED_EDGE ( 'NONE', *, *, #12589, .F. ) ;
#1206 = ADVANCED_FACE ( 'NONE', ( #5426 ), #6831, .F. ) ;
#1207 = EDGE_CURVE ( 'NONE', #8335, #9473, #5903, .T. ) ;
#1208 = LINE ( 'NONE', #5332, #2944 ) ;
#1209 = AXIS2_PLACEMENT_3D ( 'NONE', #1542, #9929, #1476 ) ;
#1210 = AXIS2_PLACEMENT_3D ( 'NONE', #424, #12838, #1323 ) ;
#1211 = AXIS2_PLACEMENT_3D ( 'NONE', #2018, #6213, #2986 ) ;
#1212 = CARTESIAN_POINT ( 'NONE',  ( -7.939678587550617728, 9.000000000000000000, 0.2057875656132798770 ) ) ;
#1213 = DIRECTION ( 'NONE',  ( 0.000000000000000000, 1.000000000000000000, 0.000000000000000000 ) ) ;
#1214 = CARTESIAN_POINT ( 'NONE',  ( 6.025412986832064277, 3.000000000000000000, -13.73660796332615597 ) ) ;
#1215 = CARTESIAN_POINT ( 'NONE',  ( -14.16466328168010769, 0.000000000000000000, -1.557181465540673271 ) ) ;
#1216 = ADVANCED_FACE ( 'NONE', ( #10172 ), #3764, .T. ) ;
#1217 = ORIENTED_EDGE ( 'NONE', *, *, #12857, .T. ) ;
#1218 = AXIS2_PLACEMENT_3D ( 'NONE', #890, #6256, #9422 ) ;
#1219 = ORIENTED_EDGE ( 'NONE', *, *, #12818, .T. ) ;
#1220 = DIRECTION ( 'NONE',  ( 0.000000000000000000, 1.000000000000000000, 0.000000000000000000 ) ) ;
#1221 = ADVANCED_FACE ( 'NONE', ( #13141 ), #3750, .F. ) ;
#1222 = ORIENTED_EDGE ( 'NONE', *, *, #12916, .F. ) ;
#1223 = CARTESIAN_POINT ( 'NONE',  ( -2.551540321038929007E-15, 0.000000000000000000, -7.000000000000000000 ) ) ;
#1224 = DIRECTION ( 'NONE',  ( -0.000000000000000000, -1.000000000000000000, -0.000000000000000000 ) ) ;
#1225 =( GEOMETRIC_REPRESENTATION_CONTEXT ( 3 ) GLOBAL_UNCERTAINTY_ASSIGNED_CONTEXT ( ( #358 ) ) GLOBAL_UNIT_ASSIGNED_CONTEXT ( ( #5230, #6331, #84 ) ) REPRESENTATION_CONTEXT ( 'NONE', 'WORKASPACE' ) );
#1226 = DIRECTION ( 'NONE',  ( 0.6291930273683290498, 0.000000000000000000, -0.7772490812545727046 ) ) ;
#1227 = CARTESIAN_POINT ( 'NONE',  ( -1.557181465540760534, 3.000000000000000000, -14.16466328168009703 ) ) ;
#1228 = CARTESIAN_POINT ( 'NONE',  ( -7.500000000000000000, 0.000000000000000000, 0.000000000000000000 ) ) ;
#1229 = EDGE_CURVE ( 'NONE', #5490, #3555, #13488, .T. ) ;
#1230 = CARTESIAN_POINT ( 'NONE',  ( -5.733772933379540859, 3.000000000000000000, -13.04554897075796660 ) ) ;
#1231 = DIRECTION ( 'NONE',  ( 0.000000000000000000, 0.000000000000000000, -1.000000000000000000 ) ) ;
#1232 = ORIENTED_EDGE ( 'NONE', *, *, #4731, .T. ) ;
#1233 = ORIENTED_EDGE ( 'NONE', *, *, #4398, .F. ) ;
#1234 = AXIS2_PLACEMENT_3D ( 'NONE', #10104, #677, #4951 ) ;
#1235 = VERTEX_POINT ( 'NONE', #750 ) ;
#1236 = DIRECTION ( 'NONE',  ( 0.000000000000000000, 0.000000000000000000, 1.000000000000000000 ) ) ;
#1237 = VERTEX_POINT ( 'NONE', #2664 ) ;
#1238 = CARTESIAN_POINT ( 'NONE',  ( 13.54609072798131209, 3.000000000000000000, 3.536018380791111415 ) ) ;
#1239 = SURFACE_SIDE_STYLE ('',( #2602 ) ) ;
#1240 = CARTESIAN_POINT ( 'NONE',  ( 0.000000000000000000, 3.000000000000000000, 0.000000000000000000 ) ) ;
#1241 = CARTESIAN_POINT ( 'NONE',  ( 5.051606143860418285, 1.734723475976807094E-15, 4.477027514692275112 ) ) ;
#1242 = CARTESIAN_POINT ( 'NONE',  ( -1.958311002203252160, 3.000000000000000000, -14.87484884897975768 ) ) ;
#1243 = CARTESIAN_POINT ( 'NONE',  ( -5.039625798601655937, 9.000000000000000000, 4.490509081392509927 ) ) ;
#1244 = CARTESIAN_POINT ( 'NONE',  ( 23.99887587215152607, 3.000000000000000000, 4.000000000000000000 ) ) ;
#1245 = ORIENTED_EDGE ( 'NONE', *, *, #13083, .F. ) ;
#1246 = CARTESIAN_POINT ( 'NONE',  ( -11.52666717836884125, 0.000000000000000000, -3.647470871583627705 ) ) ;
#1247 = VERTEX_POINT ( 'NONE', #4666 ) ;
#1248 = VERTEX_POINT ( 'NONE', #6868 ) ;
#1249 = ORIENTED_EDGE ( 'NONE', *, *, #3731, .T. ) ;
#1250 = CARTESIAN_POINT ( 'NONE',  ( 19.65244806805498001, 3.000000000000000000, -5.000000000000000000 ) ) ;
#1251 = VERTEX_POINT ( 'NONE', #6946 ) ;
#1252 = CARTESIAN_POINT ( 'NONE',  ( 0.000000000000000000, 3.000000000000000000, 0.000000000000000000 ) ) ;
#1253 = CARTESIAN_POINT ( 'NONE',  ( 4.690415759823430619, 3.000000000000000000, 1.500000000000000000 ) ) ;
#1254 = DIRECTION ( 'NONE',  ( -1.000000000000000000, 0.000000000000000000, 0.000000000000000000 ) ) ;
#1255 = CARTESIAN_POINT ( 'NONE',  ( -5.975392301194330180, 9.000000000000000000, -6.045220165289885372 ) ) ;
#1256 = EDGE_CURVE ( 'NONE', #500, #284, #294, .T. ) ;
#1257 = CARTESIAN_POINT ( 'NONE',  ( 13.50000000000000355, 3.000000000000000000, -7.050000000000000711 ) ) ;
#1258 = PLANE ( 'NONE',  #10858 ) ;
#1259 = CARTESIAN_POINT ( 'NONE',  ( 11.11702303352196708, 3.000000000000000000, 8.914835885878218846 ) ) ;
#1260 = DIRECTION ( 'NONE',  ( 0.000000000000000000, 1.000000000000000000, 0.000000000000000000 ) ) ;
#1261 = ORIENTED_EDGE ( 'NONE', *, *, #5620, .F. ) ;
#1262 = DIRECTION ( 'NONE',  ( 0.000000000000000000, 1.000000000000000000, 0.000000000000000000 ) ) ;
#1263 = PRODUCT ( 'link', 'link', '', ( #956 ) ) ;
#1264 = ORIENTED_EDGE ( 'NONE', *, *, #2886, .T. ) ;
#1265 = ORIENTED_EDGE ( 'NONE', *, *, #666, .F. ) ;
#1266 = VERTEX_POINT ( 'NONE', #11146 ) ;
#1267 = CARTESIAN_POINT ( 'NONE',  ( -0.7527353566742582824, 9.000000000000000000, 7.906594341344654886 ) ) ;
#1268 = CARTESIAN_POINT ( 'NONE',  ( 6.025412986832064277, 3.000000000000000000, -13.73660796332615597 ) ) ;
#1269 = EDGE_CURVE ( 'NONE', #9570, #11420, #3803, .T. ) ;
#1270 = EDGE_CURVE ( 'NONE', #9400, #12697, #9064, .T. ) ;
#1271 = CARTESIAN_POINT ( 'NONE',  ( 1.133238802859644956, 0.000000000000000000, -14.39763212228013600 ) ) ;
#1272 = CARTESIAN_POINT ( 'NONE',  ( -9.324917476840782982, 0.000000000000000000, -9.065441278446241924 ) ) ;
#1273 = DIRECTION ( 'NONE',  ( -1.000000000000000000, 0.000000000000000000, 0.000000000000000000 ) ) ;
#1274 = EDGE_CURVE ( 'NONE', #9473, #11839, #12226, .T. ) ;
#1275 = CYLINDRICAL_SURFACE ( 'NONE', #5106, 14.24999999999999822 ) ;
#1276 = EDGE_CURVE ( 'NONE', #2790, #9600, #6442, .T. ) ;
#1277 = ORIENTED_EDGE ( 'NONE', *, *, #11273, .T. ) ;
#1278 = VERTEX_POINT ( 'NONE', #8856 ) ;
#1279 = FACE_OUTER_BOUND ( 'NONE', #4502, .T. ) ;
#1280 = VERTEX_POINT ( 'NONE', #11075 ) ;
#1281 = LINE ( 'NONE', #10781, #3594 ) ;
#1282 = ADVANCED_FACE ( 'NONE', ( #1650 ), #6793, .F. ) ;
#1283 = FACE_OUTER_BOUND ( 'NONE', #7951, .T. ) ;
#1284 = DIRECTION ( 'NONE',  ( 0.000000000000000000, -0.000000000000000000, -1.000000000000000000 ) ) ;
#1285 = CARTESIAN_POINT ( 'NONE',  ( -6.660869762029062890, 3.000000000000000000, -11.17001010193236610 ) ) ;
#1286 = B_SPLINE_CURVE_WITH_KNOTS ( 'NONE', 2,
 ( #7443, #4476, #6606 ),
 .UNSPECIFIED., .F., .F.,
 ( 3, 3 ),
 ( 0.000000000000000000, 1.000000000000000000 ),
 .UNSPECIFIED. ) ;
#1287 = CARTESIAN_POINT ( 'NONE',  ( 8.373678438139048552, 9.000000000000000000, 1.459968977288628178 ) ) ;
#1288 = EDGE_CURVE ( 'NONE', #11402, #5247, #1374, .T. ) ;
#1289 = CARTESIAN_POINT ( 'NONE',  ( -12.38517345876401521, 0.000000000000000000, -12.42191571009144901 ) ) ;
#1290 = SURFACE_STYLE_USAGE ( .BOTH. , #12676 ) ;
#1291 = VERTEX_POINT ( 'NONE', #3631 ) ;
#1292 = ORIENTED_EDGE ( 'NONE', *, *, #7345, .T. ) ;
#1293 = ORIENTED_EDGE ( 'NONE', *, *, #3145, .F. ) ;
#1294 = ORIENTED_EDGE ( 'NONE', *, *, #11288, .F. ) ;
#1295 = CARTESIAN_POINT ( 'NONE',  ( -8.352599575481690408, 3.000000000000000000, 28.00000000000000000 ) ) ;
#1296 = VERTEX_POINT ( 'NONE', #7830 ) ;
#1297 = ADVANCED_FACE ( 'NONE', ( #5972 ), #12048, .F. ) ;
#1298 = ADVANCED_FACE ( 'NONE', ( #5763 ), #9413, .T. ) ;
#1299 = CARTESIAN_POINT ( 'NONE',  ( 10.69794375946289655, 3.000000000000000000, 7.065816209474157006 ) ) ;
#1300 = LINE ( 'NONE', #2341, #8363 ) ;
#1301 = DIRECTION ( 'NONE',  ( 0.000000000000000000, 0.000000000000000000, 1.000000000000000000 ) ) ;
#1302 = DIRECTION ( 'NONE',  ( 0.000000000000000000, 0.000000000000000000, 1.000000000000000000 ) ) ;
#1303 = ADVANCED_FACE ( 'NONE', ( #6243 ), #5149, .T. ) ;
#1304 = CARTESIAN_POINT ( 'NONE',  ( 0.000000000000000000, 9.000000000000000000, 0.000000000000000000 ) ) ;
#1305 = CARTESIAN_POINT ( 'NONE',  ( -13.17831234185052836, 3.000000000000000000, -4.227250083625696320 ) ) ;
#1306 = EDGE_LOOP ( 'NONE', ( #12592, #5558, #11855, #389 ) ) ;
#1307 = LINE ( 'NONE', #11714, #1392 ) ;
#1308 = EDGE_LOOP ( 'NONE', ( #1538, #9293, #4547, #5125 ) ) ;
#1309 = ORIENTED_EDGE ( 'NONE', *, *, #2939, .F. ) ;
#1310 = CIRCLE ( 'NONE', #1531, 1.000000000000001776 ) ;
#1311 = ORIENTED_EDGE ( 'NONE', *, *, #885, .F. ) ;
#1312 = DIRECTION ( 'NONE',  ( 0.000000000000000000, 1.000000000000000000, 0.000000000000000000 ) ) ;
#1313 = ORIENTED_EDGE ( 'NONE', *, *, #10118, .T. ) ;
#1314 = B_SPLINE_CURVE_WITH_KNOTS ( 'NONE', 2,
 ( #391, #12036, #6720 ),
 .UNSPECIFIED., .F., .F.,
 ( 3, 3 ),
 ( 0.000000000000000000, 1.000000000000000000 ),
 .UNSPECIFIED. ) ;
#1315 = ORIENTED_EDGE ( 'NONE', *, *, #6400, .F. ) ;
#1316 = EDGE_CURVE ( 'NONE', #2354, #6704, #11356, .T. ) ;
#1317 = LINE ( 'NONE', #9588, #12455 ) ;
#1318 = CIRCLE ( 'NONE', #2016, 1.500000000000001332 ) ;
#1319 = CARTESIAN_POINT ( 'NONE',  ( 4.225031457058369317E-16, 3.000000000000000000, -3.400000000000001243 ) ) ;
#1320 = DIRECTION ( 'NONE',  ( -0.000000000000000000, -1.000000000000000000, -0.000000000000000000 ) ) ;
#1321 = DIRECTION ( 'NONE',  ( -0.000000000000000000, -1.000000000000000000, -0.000000000000000000 ) ) ;
#1322 = CARTESIAN_POINT ( 'NONE',  ( -7.500000000000000000, 3.000000000000000000, 1.500000000000000666 ) ) ;
#1323 = DIRECTION ( 'NONE',  ( -0.7772490812545771455, 0.000000000000000000, -0.6291930273683233876 ) ) ;
#1324 = ORIENTED_EDGE ( 'NONE', *, *, #13353, .T. ) ;
#1325 = DIRECTION ( 'NONE',  ( -0.9288742131985401329, 0.000000000000000000, 0.3703953240185315909 ) ) ;
#1326 = ORIENTED_EDGE ( 'NONE', *, *, #3867, .F. ) ;
#1327 = ORIENTED_EDGE ( 'NONE', *, *, #8998, .F. ) ;
#1328 = ADVANCED_FACE ( 'NONE', ( #9353 ), #3014, .T. ) ;
#1329 = ORIENTED_EDGE ( 'NONE', *, *, #4134, .T. ) ;
#1330 = CARTESIAN_POINT ( 'NONE',  ( -0.8148820470561131124, 9.000000000000000000, 6.700631854488474204 ) ) ;
#1331 = CARTESIAN_POINT ( 'NONE',  ( 0.000000000000000000, 3.000000000000000000, 0.000000000000000000 ) ) ;
#1332 = APPLICATION_PROTOCOL_DEFINITION ( 'draft international standard', 'automotive_design', 1998, #1418 ) ;
#1333 = DIRECTION ( 'NONE',  ( -0.000000000000000000, -1.000000000000000000, -0.000000000000000000 ) ) ;
#1334 = AXIS2_PLACEMENT_3D ( 'NONE', #11991, #9594, #5316 ) ;
#1335 = DIRECTION ( 'NONE',  ( -0.000000000000000000, -1.000000000000000000, -0.000000000000000000 ) ) ;
#1336 = CARTESIAN_POINT ( 'NONE',  ( -13.49999999999999645, 3.000000000000000000, -7.049999999999998934 ) ) ;
#1337 = B_SPLINE_CURVE_WITH_KNOTS ( 'NONE', 3,
 ( #8936, #4809, #13213, #2810 ),
 .UNSPECIFIED., .F., .F.,
 ( 4, 4 ),
 ( 0.1276832474596304168, 1.000000000000000000 ),
 .UNSPECIFIED. ) ;
#1338 = CARTESIAN_POINT ( 'NONE',  ( -2.546103534247749600, 3.000000000000000000, 12.55526518755974585 ) ) ;
#1339 = VERTEX_POINT ( 'NONE', #4111 ) ;
#1340 = ORIENTED_EDGE ( 'NONE', *, *, #7634, .T. ) ;
#1341 = CARTESIAN_POINT ( 'NONE',  ( 3.850308450823737960, 0.000000000000000000, 5.544152309732778505 ) ) ;
#1342 = EDGE_CURVE ( 'NONE', #7762, #9987, #8243, .T. ) ;
#1343 = EDGE_CURVE ( 'NONE', #1554, #7708, #11723, .T. ) ;
#1344 = CIRCLE ( 'NONE', #914, 8.500000000000000000 ) ;
#1345 = AXIS2_PLACEMENT_3D ( 'NONE', #7820, #3415, #10926 ) ;
#1346 = B_SPLINE_CURVE_WITH_KNOTS ( 'NONE', 3,
 ( #695, #4888, #9088, #13305 ),
 .UNSPECIFIED., .F., .F.,
 ( 4, 4 ),
 ( 0.7272709309819391787, 0.7566890080396341256 ),
 .UNSPECIFIED. ) ;
#1347 = VERTEX_POINT ( 'NONE', #818 ) ;
#1348 = DIRECTION ( 'NONE',  ( 0.5610724890695777400, 0.000000000000000000, -0.8277666712360848278 ) ) ;
#1349 = B_SPLINE_CURVE_WITH_KNOTS ( 'NONE', 3,
 ( #8865, #2672, #3771, #9974 ),
 .UNSPECIFIED., .F., .F.,
 ( 4, 4 ),
 ( 0.1276832474596248101, 1.000000000000000000 ),
 .UNSPECIFIED. ) ;
#1350 = CARTESIAN_POINT ( 'NONE',  ( 7.110882674384088276, 0.000000000000000000, -3.538387050178523729 ) ) ;
#1351 = CARTESIAN_POINT ( 'NONE',  ( 0.000000000000000000, 2.900000000000000355, 1.399999999999999911 ) ) ;
#1352 = DIRECTION ( 'NONE',  ( 0.6291930273683254971, 0.000000000000000000, -0.7772490812545754801 ) ) ;
#1353 = DIRECTION ( 'NONE',  ( -0.000000000000000000, -1.000000000000000000, -0.000000000000000000 ) ) ;
#1354 = DIRECTION ( 'NONE',  ( -0.000000000000000000, -1.000000000000000000, -0.000000000000000000 ) ) ;
#1355 = VECTOR ( 'NONE', #2270, 1000.000000000000000 ) ;
#1356 = CARTESIAN_POINT ( 'NONE',  ( 2.631756770590782057, 0.000000000000000000, -14.20034848914875347 ) ) ;
#1357 = CARTESIAN_POINT ( 'NONE',  ( 4.577511697546072789, 3.000000000000000000, 12.75843939030335505 ) ) ;
#1358 = EDGE_LOOP ( 'NONE', ( #6259, #10717, #6942, #8787 ) ) ;
#1359 = EDGE_CURVE ( 'NONE', #11340, #1456, #10893, .T. ) ;
#1360 = EDGE_LOOP ( 'NONE', ( #2486, #7663, #2721, #8694 ) ) ;
#1361 = ORIENTED_EDGE ( 'NONE', *, *, #4222, .F. ) ;
#1362 = VERTEX_POINT ( 'NONE', #4171 ) ;
#1363 = CARTESIAN_POINT ( 'NONE',  ( -7.798201703419567643, 3.000000000000000000, -27.99999999999999289 ) ) ;
#1364 = ORIENTED_EDGE ( 'NONE', *, *, #9776, .F. ) ;
#1365 = ADVANCED_FACE ( 'NONE', ( #12532 ), #1682, .F. ) ;
#1366 = EDGE_CURVE ( 'NONE', #11919, #2149, #5640, .T. ) ;
#1367 = VECTOR ( 'NONE', #2475, 1000.000000000000000 ) ;
#1368 = CARTESIAN_POINT ( 'NONE',  ( 0.000000000000000000, 9.000000000000000000, 0.000000000000000000 ) ) ;
#1369 = FILL_AREA_STYLE_COLOUR ( '', #1014 ) ;
#1370 = B_SPLINE_SURFACE_WITH_KNOTS ( 'NONE', 3, 1, ( 
 ( #5624, #9822 ),
 ( #536, #4591 ),
 ( #12042, #8847 ),
 ( #8776, #13068 ) ),
 .UNSPECIFIED., .F., .F., .F.,
 ( 4, 4 ),
 ( 2, 2 ),
 ( 0.000000000000000000, 0.5855695330273008592 ),
 ( 0.000000000000000000, 1.000000000000000000 ),
 .UNSPECIFIED. ) ;
#1371 = CARTESIAN_POINT ( 'NONE',  ( -5.733772933379540859, 3.000000000000000000, -13.04554897075796660 ) ) ;
#1372 = DIRECTION ( 'NONE',  ( -0.000000000000000000, -1.000000000000000000, -0.000000000000000000 ) ) ;
#1373 = DIRECTION ( 'NONE',  ( 0.000000000000000000, 1.000000000000000000, 0.000000000000000000 ) ) ;
#1374 = B_SPLINE_CURVE_WITH_KNOTS ( 'NONE', 2,
 ( #2805, #7013, #1778 ),
 .UNSPECIFIED., .F., .F.,
 ( 3, 3 ),
 ( 0.000000000000000000, 1.000000000000000000 ),
 .UNSPECIFIED. ) ;
#1375 = DIRECTION ( 'NONE',  ( 0.000000000000000000, 0.000000000000000000, -1.000000000000000000 ) ) ;
#1376 = ORIENTED_EDGE ( 'NONE', *, *, #4336, .T. ) ;
#1377 = VECTOR ( 'NONE', #711, 1000.000000000000000 ) ;
#1378 = ORIENTED_EDGE ( 'NONE', *, *, #7513, .T. ) ;
#1379 = AXIS2_PLACEMENT_3D ( 'NONE', #6970, #9916, #13027 ) ;
#1380 = AXIS2_PLACEMENT_3D ( 'NONE', #2769, #13035, #1743 ) ;
#1381 = ADVANCED_FACE ( 'NONE', ( #4755 ), #13486, .T. ) ;
#1382 = ORIENTED_EDGE ( 'NONE', *, *, #1952, .F. ) ;
#1383 = VERTEX_POINT ( 'NONE', #6116 ) ;
#1384 = DIRECTION ( 'NONE',  ( 0.000000000000000000, 1.000000000000000000, 0.000000000000000000 ) ) ;
#1385 = B_SPLINE_CURVE_WITH_KNOTS ( 'NONE', 3,
 ( #4618, #8805, #3586, #7305 ),
 .UNSPECIFIED., .F., .F.,
 ( 4, 4 ),
 ( 0.000000000000000000, 0.5855695330273008592 ),
 .UNSPECIFIED. ) ;
#1386 = ORIENTED_EDGE ( 'NONE', *, *, #11832, .T. ) ;
#1387 = ORIENTED_EDGE ( 'NONE', *, *, #4398, .T. ) ;
#1388 = CARTESIAN_POINT ( 'NONE',  ( -12.98835496148321944, 3.000000000000000000, -0.5501230721522550882 ) ) ;
#1389 = AXIS2_PLACEMENT_3D ( 'NONE', #12610, #3225, #12545 ) ;
#1390 =( NAMED_UNIT ( * ) PLANE_ANGLE_UNIT ( ) SI_UNIT ( $, .RADIAN. ) );
#1391 = AXIS2_PLACEMENT_3D ( 'NONE', #11674, #9545, #6166 ) ;
#1392 = VECTOR ( 'NONE', #4408, 1000.000000000000000 ) ;
#1393 = CARTESIAN_POINT ( 'NONE',  ( -12.68816982652953840, 3.000000000000000000, -2.830255545554093644 ) ) ;
#1394 = CYLINDRICAL_SURFACE ( 'NONE', #1105, 3.500000000000000888 ) ;
#1395 = AXIS2_PLACEMENT_3D ( 'NONE', #11099, #6753, #631 ) ;
#1396 = DIRECTION ( 'NONE',  ( -0.000000000000000000, -1.000000000000000000, -0.000000000000000000 ) ) ;
#1397 = CARTESIAN_POINT ( 'NONE',  ( -0.8776997859584816375, 0.000000000000000000, 7.310603390113379341 ) ) ;
#1398 = LINE ( 'NONE', #234, #998 ) ;
#1399 = ORIENTED_EDGE ( 'NONE', *, *, #4811, .F. ) ;
#1400 = CARTESIAN_POINT ( 'NONE',  ( 1.836970198721030181E-16, 0.09999999999999982514, 1.500000000000000222 ) ) ;
#1401 = EDGE_CURVE ( 'NONE', #12205, #5887, #5126, .T. ) ;
#1402 = EDGE_LOOP ( 'NONE', ( #8548, #4333, #2553, #7011 ) ) ;
#1403 = ADVANCED_FACE ( 'NONE', ( #3137 ), #3672, .T. ) ;
#1404 = VECTOR ( 'NONE', #9043, 1000.000000000000000 ) ;
#1405 = PRODUCT_DEFINITION_SHAPE ( 'NONE', 'NONE',  #13610 ) ;
#1406 = VERTEX_POINT ( 'NONE', #11126 ) ;
#1407 = VECTOR ( 'NONE', #12704, 1000.000000000000000 ) ;
#1408 = VECTOR ( 'NONE', #8380, 1000.000000000000000 ) ;
#1409 = VERTEX_POINT ( 'NONE', #12093 ) ;
#1410 = DIRECTION ( 'NONE',  ( 0.000000000000000000, 1.000000000000000000, 0.000000000000000000 ) ) ;
#1411 = CARTESIAN_POINT ( 'NONE',  ( 0.000000000000000000, 3.000000000000000000, 0.000000000000000000 ) ) ;
#1412 = CIRCLE ( 'NONE', #7350, 12.08999999999737618 ) ;
#1413 = CARTESIAN_POINT ( 'NONE',  ( 8.481367827640703183, 9.000000000000000000, 0.5624942419805130100 ) ) ;
#1414 = TOROIDAL_SURFACE ( 'NONE', #10652, 1.600000000000004086, 0.1000000000000000056 ) ;
#1415 = CARTESIAN_POINT ( 'NONE',  ( 6.025412986832064277, 0.000000000000000000, -13.73660796332615597 ) ) ;
#1416 = DIRECTION ( 'NONE',  ( -0.000000000000000000, -1.000000000000000000, -0.000000000000000000 ) ) ;
#1417 = CARTESIAN_POINT ( 'NONE',  ( -14.08504230442587790, 3.000000000000000000, -2.161962830978695571 ) ) ;
#1418 = APPLICATION_CONTEXT ( 'automotive_design' ) ;
#1419 = VERTEX_POINT ( 'NONE', #4785 ) ;
#1420 = ORIENTED_EDGE ( 'NONE', *, *, #753, .T. ) ;
#1421 = CARTESIAN_POINT ( 'NONE',  ( 9.250000000000001776, 1.999999999999998224, -10.00000000000000178 ) ) ;
#1422 = CIRCLE ( 'NONE', #5602, 4.390701948131951582 ) ;
#1423 = AXIS2_PLACEMENT_3D ( 'NONE', #9152, #9363, #12411 ) ;
#1424 = VECTOR ( 'NONE', #487, 1000.000000000000000 ) ;
#1425 = ORIENTED_EDGE ( 'NONE', *, *, #3705, .F. ) ;
#1426 = CARTESIAN_POINT ( 'NONE',  ( 31.00000000000000000, 2.900000000000000355, 0.000000000000000000 ) ) ;
#1427 = CARTESIAN_POINT ( 'NONE',  ( 8.430890348300625448, 0.000000000000000000, 11.48836750521723893 ) ) ;
#1428 = CARTESIAN_POINT ( 'NONE',  ( 30.79786191028635400, 3.000000000000000000, -7.999232361977356653 ) ) ;
#1429 = CARTESIAN_POINT ( 'NONE',  ( 1.580708947611199511, 0.000000000000000000, -8.351727918397596540 ) ) ;
#1430 = CARTESIAN_POINT ( 'NONE',  ( 0.000000000000000000, 0.000000000000000000, 0.000000000000000000 ) ) ;
#1431 = ADVANCED_FACE ( 'NONE', ( #2640 ), #1832, .T. ) ;
#1432 = VECTOR ( 'NONE', #10143, 1000.000000000000000 ) ;
#1433 = FACE_OUTER_BOUND ( 'NONE', #9405, .T. ) ;
#1434 = VECTOR ( 'NONE', #1043, 1000.000000000000000 ) ;
#1435 = DIRECTION ( 'NONE',  ( -1.000000000000000000, 0.000000000000000000, -0.000000000000000000 ) ) ;
#1436 = ORIENTED_EDGE ( 'NONE', *, *, #1948, .F. ) ;
#1437 = VERTEX_POINT ( 'NONE', #653 ) ;
#1438 = ORIENTED_EDGE ( 'NONE', *, *, #4998, .F. ) ;
#1439 = ORIENTED_EDGE ( 'NONE', *, *, #8319, .F. ) ;
#1440 = LINE ( 'NONE', #9630, #11953 ) ;
#1441 = VERTEX_POINT ( 'NONE', #1624 ) ;
#1442 = PRESENTATION_LAYER_ASSIGNMENT (  '', '', ( #2987 ) ) ;
#1443 = AXIS2_PLACEMENT_3D ( 'NONE', #11916, #10885, #1450 ) ;
#1444 = CARTESIAN_POINT ( 'NONE',  ( -4.334442004268530546, 9.000000000000000000, 7.311813216407585081 ) ) ;
#1445 = EDGE_CURVE ( 'NONE', #11616, #8766, #4718, .T. ) ;
#1446 = CARTESIAN_POINT ( 'NONE',  ( 0.000000000000000000, 9.000000000000000000, 0.000000000000000000 ) ) ;
#1447 = EDGE_CURVE ( 'NONE', #8041, #9479, #13283, .T. ) ;
#1448 = CARTESIAN_POINT ( 'NONE',  ( -8.479748006907131597, 0.000000000000000000, 0.5864074857593127854 ) ) ;
#1449 = CARTESIAN_POINT ( 'NONE',  ( 8.158551673544288008, 0.000000000000000000, -8.922226997226886169 ) ) ;
#1450 = DIRECTION ( 'NONE',  ( 0.000000000000000000, 0.000000000000000000, -1.000000000000000000 ) ) ;
#1451 = ORIENTED_EDGE ( 'NONE', *, *, #8998, .T. ) ;
#1452 = AXIS2_PLACEMENT_3D ( 'NONE', #4539, #11912, #3565 ) ;
#1453 = EDGE_CURVE ( 'NONE', #3691, #11432, #13398, .T. ) ;
#1454 =( NAMED_UNIT ( * ) SI_UNIT ( $, .STERADIAN. ) SOLID_ANGLE_UNIT ( ) );
#1455 = EDGE_CURVE ( 'NONE', #3087, #8384, #6921, .T. ) ;
#1456 = VERTEX_POINT ( 'NONE', #592 ) ;
#1457 = PRODUCT_DEFINITION_CONTEXT ( 'detailed design', #12167, 'design' ) ;
#1458 = ORIENTED_EDGE ( 'NONE', *, *, #8658, .F. ) ;
#1459 = DIRECTION ( 'NONE',  ( 2.602085213965199795E-16, -2.891205793294684736E-16, 1.000000000000000000 ) ) ;
#1460 = ORIENTED_EDGE ( 'NONE', *, *, #6068, .F. ) ;
#1461 = ORIENTED_EDGE ( 'NONE', *, *, #11441, .T. ) ;
#1462 = LINE ( 'NONE', #12068, #9122 ) ;
#1463 = CARTESIAN_POINT ( 'NONE',  ( 0.000000000000000000, 0.000000000000000000, 0.000000000000000000 ) ) ;
#1464 = CARTESIAN_POINT ( 'NONE',  ( -13.27898586450066709, 3.000000000000000000, 5.170206418547661720 ) ) ;
#1465 = ADVANCED_FACE ( 'NONE', ( #5950 ), #13260, .F. ) ;
#1466 = CARTESIAN_POINT ( 'NONE',  ( 0.9098489087730803337, 9.000000000000000000, 7.307220250892556557 ) ) ;
#1467 = FACE_BOUND ( 'NONE', #10598, .T. ) ;
#1468 = CARTESIAN_POINT ( 'NONE',  ( -12.68816982652953840, 3.000000000000000000, -2.830255545554093644 ) ) ;
#1469 = CARTESIAN_POINT ( 'NONE',  ( 31.00000000000000000, 0.09999999999999982514, 0.000000000000000000 ) ) ;
#1470 = ORIENTED_EDGE ( 'NONE', *, *, #8368, .T. ) ;
#1471 = DIRECTION ( 'NONE',  ( 0.000000000000000000, 0.000000000000000000, 1.000000000000000000 ) ) ;
#1472 = EDGE_LOOP ( 'NONE', ( #7725, #6948, #2931, #9761 ) ) ;
#1473 = ORIENTED_EDGE ( 'NONE', *, *, #141, .T. ) ;
#1474 = ORIENTED_EDGE ( 'NONE', *, *, #6168, .F. ) ;
#1475 = CARTESIAN_POINT ( 'NONE',  ( 47.14458624375820506, 0.000000000000000000, -3.829406728833672613 ) ) ;
#1476 = DIRECTION ( 'NONE',  ( 0.000000000000000000, 0.000000000000000000, -1.000000000000000000 ) ) ;
#1477 = EDGE_CURVE ( 'NONE', #10812, #4058, #6302, .T. ) ;
#1478 = EDGE_CURVE ( 'NONE', #2415, #12329, #10151, .T. ) ;
#1479 = DIRECTION ( 'NONE',  ( -0.000000000000000000, -1.000000000000000000, -0.000000000000000000 ) ) ;
#1480 = CARTESIAN_POINT ( 'NONE',  ( 0.5501230721522984979, 0.000000000000000000, -12.98835496148321766 ) ) ;
#1481 = DIRECTION ( 'NONE',  ( 0.000000000000000000, 0.000000000000000000, 1.000000000000000000 ) ) ;
#1482 = CARTESIAN_POINT ( 'NONE',  ( 7.077546079049268357, 0.000000000000000000, 10.67828022838850544 ) ) ;
#1483 = CARTESIAN_POINT ( 'NONE',  ( 0.000000000000000000, 9.000000000000000000, 0.000000000000000000 ) ) ;
#1484 = EDGE_LOOP ( 'NONE', ( #1936, #11700, #6849, #341 ) ) ;
#1485 = ORIENTED_EDGE ( 'NONE', *, *, #10916, .T. ) ;
#1486 = B_SPLINE_SURFACE_WITH_KNOTS ( 'NONE', 3, 1, ( 
 ( #8264, #973 ),
 ( #9432, #4193 ),
 ( #776, #4969 ),
 ( #13377, #9164 ) ),
 .UNSPECIFIED., .F., .F., .F.,
 ( 4, 4 ),
 ( 2, 2 ),
 ( 0.000000000000000000, 0.5855695330273008592 ),
 ( 0.000000000000000000, 1.000000000000000000 ),
 .UNSPECIFIED. ) ;
#1487 = ORIENTED_EDGE ( 'NONE', *, *, #4130, .T. ) ;
#1488 = CARTESIAN_POINT ( 'NONE',  ( 31.00000000000000000, 0.000000000000000000, 3.999999998926329514 ) ) ;
#1489 = DIRECTION ( 'NONE',  ( -0.6204948238377417935, -0.000000000000000000, 0.7842105416216806901 ) ) ;
#1490 = B_SPLINE_CURVE_WITH_KNOTS ( 'NONE', 3,
 ( #12693, #9306, #7309, #3097 ),
 .UNSPECIFIED., .F., .F.,
 ( 4, 4 ),
 ( 0.1547128134717859205, 1.000000000000000000 ),
 .UNSPECIFIED. ) ;
#1491 = DIRECTION ( 'NONE',  ( -1.000000000000000000, 0.000000000000000000, 0.000000000000000000 ) ) ;
#1492 = CARTESIAN_POINT ( 'NONE',  ( -13.50845331674225847, 0.000000000000000000, 1.119409668803372115 ) ) ;
#1493 = DIRECTION ( 'NONE',  ( -0.000000000000000000, -1.000000000000000000, -0.000000000000000000 ) ) ;
#1494 = CARTESIAN_POINT ( 'NONE',  ( -7.235926821844430812, 9.000000000000000000, 4.459973433655439301 ) ) ;
#1495 = B_SPLINE_CURVE_WITH_KNOTS ( 'NONE', 3,
 ( #378, #6768, #3806, #3599 ),
 .UNSPECIFIED., .F., .F.,
 ( 4, 4 ),
 ( 0.1276832474596284739, 1.000000000000000000 ),
 .UNSPECIFIED. ) ;
#1496 = DIRECTION ( 'NONE',  ( 0.000000000000000000, 1.000000000000000000, 0.000000000000000000 ) ) ;
#1497 = DIRECTION ( 'NONE',  ( -0.000000000000000000, -1.000000000000000000, -0.000000000000000000 ) ) ;
#1498 = ORIENTED_EDGE ( 'NONE', *, *, #2054, .F. ) ;
#1499 = ORIENTED_EDGE ( 'NONE', *, *, #9261, .F. ) ;
#1500 = EDGE_LOOP ( 'NONE', ( #6553, #10140, #4999, #10132 ) ) ;
#1501 = VERTEX_POINT ( 'NONE', #5885 ) ;
#1502 = CARTESIAN_POINT ( 'NONE',  ( 0.000000000000000000, 0.000000000000000000, 0.000000000000000000 ) ) ;
#1503 = ADVANCED_FACE ( 'NONE', ( #2924 ), #725, .T. ) ;
#1504 = EDGE_LOOP ( 'NONE', ( #1890, #2339, #249, #3 ) ) ;
#1505 = CYLINDRICAL_SURFACE ( 'NONE', #12322, 1.499999999999999556 ) ;
#1506 = SURFACE_STYLE_FILL_AREA ( #6798 ) ;
#1507 = CARTESIAN_POINT ( 'NONE',  ( 20.00000000000000711, 3.000000000000000000, 12.57924256039204280 ) ) ;
#1508 = FACE_BOUND ( 'NONE', #561, .T. ) ;
#1509 = CARTESIAN_POINT ( 'NONE',  ( 5.967832595844252630, 0.000000000000000000, -3.153961652902406154 ) ) ;
#1510 = PRODUCT_DEFINITION_SHAPE ( 'NONE', 'NONE',  #13614 ) ;
#1511 = CARTESIAN_POINT ( 'NONE',  ( 29.39270799701850123, 3.000000000000000000, -0.3930766723116408401 ) ) ;
#1512 = FACE_OUTER_BOUND ( 'NONE', #6478, .T. ) ;
#1513 = VERTEX_POINT ( 'NONE', #6993 ) ;
#1514 = DIRECTION ( 'NONE',  ( 0.000000000000000000, 0.000000000000000000, -1.000000000000000000 ) ) ;
#1515 = VERTEX_POINT ( 'NONE', #7874 ) ;
#1516 = ORIENTED_EDGE ( 'NONE', *, *, #12315, .T. ) ;
#1517 = CARTESIAN_POINT ( 'NONE',  ( -13.00394681030572208, 0.000000000000000000, -0.1834665838397169235 ) ) ;
#1518 = ADVANCED_FACE ( 'NONE', ( #9124 ), #2773, .F. ) ;
#1519 = ADVANCED_FACE ( 'NONE', ( #13186 ), #3739, .T. ) ;
#1520 = ORIENTED_EDGE ( 'NONE', *, *, #10883, .F. ) ;
#1521 = EDGE_CURVE ( 'NONE', #3318, #464, #2714, .T. ) ;
#1522 = EDGE_CURVE ( 'NONE', #7238, #10060, #4127, .T. ) ;
#1523 = ORIENTED_EDGE ( 'NONE', *, *, #12902, .T. ) ;
#1524 = B_SPLINE_CURVE_WITH_KNOTS ( 'NONE', 3,
 ( #12864, #7682, #390, #9619 ),
 .UNSPECIFIED., .F., .F.,
 ( 4, 4 ),
 ( 0.000000000000000000, 0.5855695330273008592 ),
 .UNSPECIFIED. ) ;
#1525 = CARTESIAN_POINT ( 'NONE',  ( 0.000000000000000000, 3.000000000000000000, 0.000000000000000000 ) ) ;
#1526 = EDGE_CURVE ( 'NONE', #12590, #8924, #3816, .T. ) ;
#1527 = CARTESIAN_POINT ( 'NONE',  ( -12.14623037080100865, 3.000000000000000000, 4.072642252455982437 ) ) ;
#1528 = CARTESIAN_POINT ( 'NONE',  ( 0.000000000000000000, 3.000000000000000000, 0.000000000000000000 ) ) ;
#1529 = CARTESIAN_POINT ( 'NONE',  ( 9.065480927540312095, 0.000000000000000000, -9.324856600128422102 ) ) ;
#1530 = CARTESIAN_POINT ( 'NONE',  ( 2.161962830978677363, 3.000000000000000000, 14.08504230442587613 ) ) ;
#1531 = AXIS2_PLACEMENT_3D ( 'NONE', #1238, #4264, #5428 ) ;
#1532 = CYLINDRICAL_SURFACE ( 'NONE', #6265, 1.500000000000001332 ) ;
#1533 = ORIENTED_EDGE ( 'NONE', *, *, #12497, .F. ) ;
#1534 = DIRECTION ( 'NONE',  ( 0.000000000000000000, 0.000000000000000000, 1.000000000000000000 ) ) ;
#1535 = VERTEX_POINT ( 'NONE', #5152 ) ;
#1536 = VERTEX_POINT ( 'NONE', #7032 ) ;
#1537 = EDGE_CURVE ( 'NONE', #13428, #13474, #4113, .T. ) ;
#1538 = ORIENTED_EDGE ( 'NONE', *, *, #12078, .T. ) ;
#1539 = AXIS2_PLACEMENT_3D ( 'NONE', #10224, #11328, #797 ) ;
#1540 = CARTESIAN_POINT ( 'NONE',  ( 4.355042381134428098, 0.000000000000000000, 7.299562031966232212 ) ) ;
#1541 = EDGE_CURVE ( 'NONE', #10087, #357, #309, .T. ) ;
#1542 = CARTESIAN_POINT ( 'NONE',  ( 0.000000000000000000, 2.900000000000000355, -1.399999999999999911 ) ) ;
#1543 = EDGE_CURVE ( 'NONE', #7533, #13228, #1801, .T. ) ;
#1544 = CARTESIAN_POINT ( 'NONE',  ( 6.951477219042924816, 0.000000000000000000, 3.842108769784387423 ) ) ;
#1545 = DIRECTION ( 'NONE',  ( 1.000000000000000000, -3.469446951953610639E-15, -2.602085213965210149E-16 ) ) ;
#1546 = CONTEXT_DEPENDENT_SHAPE_REPRESENTATION ( #9602, #8526 ) ;
#1547 = DIRECTION ( 'NONE',  ( 0.000000000000000000, 0.000000000000000000, 1.000000000000000000 ) ) ;
#1548 = FACE_OUTER_BOUND ( 'NONE', #9846, .T. ) ;
#1549 = FACE_BOUND ( 'NONE', #2100, .T. ) ;
#1550 = CARTESIAN_POINT ( 'NONE',  ( 5.250000000000000000, 3.000000000000000000, -27.94078293894052578 ) ) ;
#1551 = CIRCLE ( 'NONE', #9238, 3.499999999999999556 ) ;
#1552 = AXIS2_PLACEMENT_3D ( 'NONE', #10406, #12287, #12356 ) ;
#1553 = ORIENTED_EDGE ( 'NONE', *, *, #10207, .T. ) ;
#1554 = VERTEX_POINT ( 'NONE', #11563 ) ;
#1555 = EDGE_CURVE ( 'NONE', #12329, #2013, #3150, .T. ) ;
#1557 = ORIENTED_EDGE ( 'NONE', *, *, #5493, .F. ) ;
#1556 = B_SPLINE_CURVE_WITH_KNOTS ( 'NONE', 3,
 ( #3713, #1527, #1595, #1464 ),
 .UNSPECIFIED., .F., .F.,
 ( 4, 4 ),
 ( 0.1547128134717859205, 1.000000000000000000 ),
 .UNSPECIFIED. ) ;
#1558 = CARTESIAN_POINT ( 'NONE',  ( -1.650143266773857142, 0.000000000000000000, -14.90895795148409952 ) ) ;
#1559 = DIRECTION ( 'NONE',  ( 0.000000000000000000, 1.000000000000000000, 0.000000000000000000 ) ) ;
#1560 = AXIS2_PLACEMENT_3D ( 'NONE', #9654, #5449, #13085 ) ;
#1561 = AXIS2_PLACEMENT_3D ( 'NONE', #6857, #455, #6785 ) ;
#1562 = CARTESIAN_POINT ( 'NONE',  ( -10.34346111134701118, 3.000000000000000000, -8.760376775873707444 ) ) ;
#1563 = CARTESIAN_POINT ( 'NONE',  ( 11.11702303352196708, 3.000000000000000000, 8.914835885878218846 ) ) ;
#1564 = CARTESIAN_POINT ( 'NONE',  ( 22.00000000000000000, 3.000000000000000000, -1.500000000000000666 ) ) ;
#1565 = CARTESIAN_POINT ( 'NONE',  ( 0.4639228963249696913, 9.000000000000000000, 8.487330295579727846 ) ) ;
#1566 = CARTESIAN_POINT ( 'NONE',  ( -13.61374091949023679, 3.000000000000000000, -4.821006024660923650 ) ) ;
#1567 = ORIENTED_EDGE ( 'NONE', *, *, #11702, .F. ) ;
#1568 = AXIS2_PLACEMENT_3D ( 'NONE', #12469, #12655, #8432 ) ;
#1569 = EDGE_CURVE ( 'NONE', #5437, #5898, #5276, .T. ) ;
#1570 = ORIENTED_EDGE ( 'NONE', *, *, #2217, .F. ) ;
#1571 = AXIS2_PLACEMENT_3D ( 'NONE', #1768, #5267, #11551 ) ;
#1572 = ORIENTED_EDGE ( 'NONE', *, *, #10096, .T. ) ;
#1573 = DIRECTION ( 'NONE',  ( -1.000000000000000000, 0.000000000000000000, -0.000000000000000000 ) ) ;
#1574 = ORIENTED_EDGE ( 'NONE', *, *, #1526, .F. ) ;
#1575 = EDGE_CURVE ( 'NONE', #6867, #8751, #9965, .T. ) ;
#1576 = DIRECTION ( 'NONE',  ( -0.000000000000000000, -1.000000000000000000, -0.000000000000000000 ) ) ;
#1577 = DIRECTION ( 'NONE',  ( 1.000000000000000000, 0.000000000000000000, 0.000000000000000000 ) ) ;
#1578 = CARTESIAN_POINT ( 'NONE',  ( 26.30958424017656938, 0.09999999999999982514, -4.500000000000000888 ) ) ;
#1579 = DIRECTION ( 'NONE',  ( 0.000000000000000000, 0.000000000000000000, 1.000000000000000000 ) ) ;
#1580 = CARTESIAN_POINT ( 'NONE',  ( -5.975392301194330180, 9.000000000000000000, -6.045220165289885372 ) ) ;
#1581 = CARTESIAN_POINT ( 'NONE',  ( 0.000000000000000000, 0.000000000000000000, 0.000000000000000000 ) ) ;
#1582 = FACE_OUTER_BOUND ( 'NONE', #2814, .T. ) ;
#1583 = ADVANCED_FACE ( 'NONE', ( #10520 ), #12251, .F. ) ;
#1584 = VERTEX_POINT ( 'NONE', #1667 ) ;
#1585 = ORIENTED_EDGE ( 'NONE', *, *, #8385, .F. ) ;
#1586 = UNCERTAINTY_MEASURE_WITH_UNIT (LENGTH_MEASURE( 1.000000000000000082E-05 ), #6895, 'distance_accuracy_value', 'NONE');
#1587 = VECTOR ( 'NONE', #7081, 1000.000000000000000 ) ;
#1588 = ORIENTED_EDGE ( 'NONE', *, *, #788, .F. ) ;
#1589 = LINE ( 'NONE', #3857, #4670 ) ;
#1590 = CIRCLE ( 'NONE', #9283, 3.499999999999999556 ) ;
#1591 = ORIENTED_EDGE ( 'NONE', *, *, #7324, .F. ) ;
#1592 = VERTEX_POINT ( 'NONE', #12597 ) ;
#1593 = FACE_OUTER_BOUND ( 'NONE', #5258, .T. ) ;
#1594 =( REPRESENTATION_RELATIONSHIP ('NONE','NONE', #3798, #8539 ) REPRESENTATION_RELATIONSHIP_WITH_TRANSFORMATION ( #4573 )SHAPE_REPRESENTATION_RELATIONSHIP( ) );
#1595 = CARTESIAN_POINT ( 'NONE',  ( -12.75843939030334795, 3.000000000000000000, 4.577511697546079006 ) ) ;
#1596 = CARTESIAN_POINT ( 'NONE',  ( 1.119409668803368119, 0.000000000000000000, 13.50845331674225847 ) ) ;
#1597 = VECTOR ( 'NONE', #7587, 1000.000000000000000 ) ;
#1598 = DIRECTION ( 'NONE',  ( 0.000000000000000000, 0.000000000000000000, 1.000000000000000000 ) ) ;
#1599 = CIRCLE ( 'NONE', #4671, 6.750000000000000888 ) ;
#1600 = CIRCLE ( 'NONE', #7756, 2.999999999999999112 ) ;
#1601 = FACE_OUTER_BOUND ( 'NONE', #9061, .T. ) ;
#1602 = DIRECTION ( 'NONE',  ( 0.000000000000000000, 0.000000000000000000, 1.000000000000000000 ) ) ;
#1603 = ADVANCED_FACE ( 'NONE', ( #4822 ), #13559, .T. ) ;
#1604 = ORIENTED_EDGE ( 'NONE', *, *, #11034, .F. ) ;
#1605 = PRODUCT_DEFINITION ( 'UNKNOWN', '', #8267, #12345 ) ;
#1606 = FACE_OUTER_BOUND ( 'NONE', #1630, .T. ) ;
#1607 = B_SPLINE_SURFACE_WITH_KNOTS ( 'NONE', 3, 1, ( 
 ( #7924, #2832 ),
 ( #9920, #3719 ),
 ( #8889, #11106 ),
 ( #4973, #6974 ) ),
 .UNSPECIFIED., .F., .F., .F.,
 ( 4, 4 ),
 ( 2, 2 ),
 ( 0.1547128134717859205, 1.000000000000000000 ),
 ( 0.000000000000000000, 1.000000000000000000 ),
 .UNSPECIFIED. ) ;
#1608 = VERTEX_POINT ( 'NONE', #10196 ) ;
#1609 = ORIENTED_EDGE ( 'NONE', *, *, #2578, .F. ) ;
#1610 = ORIENTED_EDGE ( 'NONE', *, *, #1879, .T. ) ;
#1611 = AXIS2_PLACEMENT_3D ( 'NONE', #2050, #7158, #8369 ) ;
#1612 = AXIS2_PLACEMENT_3D ( 'NONE', #5175, #8323, #10405 ) ;
#1613 = AXIS2_PLACEMENT_3D ( 'NONE', #13583, #19, #10548 ) ;
#1614 = DIRECTION ( 'NONE',  ( 0.000000000000000000, 0.000000000000000000, -1.000000000000000000 ) ) ;
#1615 = CARTESIAN_POINT ( 'NONE',  ( 10.98198414889934682, 0.000000000000000000, -9.379342464487748998 ) ) ;
#1616 = DIRECTION ( 'NONE',  ( -0.000000000000000000, -1.000000000000000000, -0.000000000000000000 ) ) ;
#1617 = FACE_OUTER_BOUND ( 'NONE', #13568, .T. ) ;
#1618 = DIRECTION ( 'NONE',  ( 0.000000000000000000, 1.000000000000000000, 0.000000000000000000 ) ) ;
#1619 = CARTESIAN_POINT ( 'NONE',  ( -9.065441275458884007, 0.000000000000000000, -9.324917484779556176 ) ) ;
#1620 = EDGE_CURVE ( 'NONE', #1235, #3720, #13225, .T. ) ;
#1621 = CARTESIAN_POINT ( 'NONE',  ( 20.00000000000001421, 5.999999999999972466, -5.204170427930418128E-15 ) ) ;
#1622 = FACE_BOUND ( 'NONE', #4217, .T. ) ;
#1623 = VECTOR ( 'NONE', #2118, 1000.000000000000000 ) ;
#1624 = CARTESIAN_POINT ( 'NONE',  ( 8.795158114916441505, 3.000000000000000000, -9.573149624528689117 ) ) ;
#1625 = CARTESIAN_POINT ( 'NONE',  ( -8.479748006907131597, 9.000000000000000000, 0.5864074857593127854 ) ) ;
#1626 = AXIS2_PLACEMENT_3D ( 'NONE', #11875, #9668, #5531 ) ;
#1627 = AXIS2_PLACEMENT_3D ( 'NONE', #11632, #9626, #8578 ) ;
#1628 = EDGE_LOOP ( 'NONE', ( #967, #8471, #2768, #4879 ) ) ;
#1629 = ADVANCED_FACE ( 'NONE', ( #3784 ), #8372, .F. ) ;
#1630 = EDGE_LOOP ( 'NONE', ( #9979, #6504, #3840, #12459, #9427, #11054, #12260, #11882, #1794, #1294, #6593, #5923, #12223, #9618, #6732, #1311, #5467, #13454, #10169, #1160, #8458, #5363, #5414, #7618, #8830, #3725, #12842 ) ) ;
#1631 = EDGE_CURVE ( 'NONE', #8075, #1251, #9534, .T. ) ;
#1632 = ORIENTED_EDGE ( 'NONE', *, *, #5222, .T. ) ;
#1633 = CARTESIAN_POINT ( 'NONE',  ( 8.922136023539611216, 3.000000000000000000, -8.158651161643899030 ) ) ;
#1634 = VECTOR ( 'NONE', #7068, 1000.000000000000000 ) ;
#1635 = VECTOR ( 'NONE', #8325, 1000.000000000000000 ) ;
#1636 = CARTESIAN_POINT ( 'NONE',  ( 45.60964950616533287, 0.000000000000000000, -14.50984893380129392 ) ) ;
#1637 = FACE_OUTER_BOUND ( 'NONE', #7799, .T. ) ;
#1638 = EDGE_CURVE ( 'NONE', #12749, #2659, #1346, .T. ) ;
#1639 = CARTESIAN_POINT ( 'NONE',  ( 0.8327827707325454742, 0.000000000000000000, 6.698430626405788679 ) ) ;
#1640 = CARTESIAN_POINT ( 'NONE',  ( -2.830255545554292151, 3.000000000000000000, -12.68816982652971959 ) ) ;
#1641 = FACE_OUTER_BOUND ( 'NONE', #8618, .T. ) ;
#1642 = DIRECTION ( 'NONE',  ( -1.000000000000000000, -0.000000000000000000, 1.055752450943286591E-16 ) ) ;
#1643 = CIRCLE ( 'NONE', #10868, 8.499999999999996447 ) ;
#1644 = CARTESIAN_POINT ( 'NONE',  ( 12.03251085770905959, 3.000000000000000000, 3.999999998926332179 ) ) ;
#1645 = AXIS2_PLACEMENT_3D ( 'NONE', #9835, #7977, #5911 ) ;
#1646 = ORIENTED_EDGE ( 'NONE', *, *, #7221, .T. ) ;
#1647 = ADVANCED_FACE ( 'NONE', ( #10123 ), #7992, .T. ) ;
#1648 = EDGE_LOOP ( 'NONE', ( #5645, #712, #3236, #11092 ) ) ;
#1649 = ORIENTED_EDGE ( 'NONE', *, *, #10971, .F. ) ;
#1650 = FACE_OUTER_BOUND ( 'NONE', #4981, .T. ) ;
#1651 = VERTEX_POINT ( 'NONE', #9558 ) ;
#1652 = CARTESIAN_POINT ( 'NONE',  ( -2.604531154829235362, 3.000000000000000000, -11.80612203322752585 ) ) ;
#1653 = DIRECTION ( 'NONE',  ( 0.000000000000000000, 0.000000000000000000, 1.000000000000000000 ) ) ;
#1654 = VECTOR ( 'NONE', #5931, 1000.000000000000000 ) ;
#1655 = EDGE_CURVE ( 'NONE', #8384, #1142, #4469, .T. ) ;
#1656 = CARTESIAN_POINT ( 'NONE',  ( 13.04554897075798081, 3.000000000000000000, -5.733772933379503556 ) ) ;
#1657 = CARTESIAN_POINT ( 'NONE',  ( -6.721397655168936502, 9.000000000000000000, 5.203154193476255074 ) ) ;
#1658 = CARTESIAN_POINT ( 'NONE',  ( -5.526615004551211463, 9.000000000000000000, -4.866191470063547797 ) ) ;
#1659 = CARTESIAN_POINT ( 'NONE',  ( 0.000000000000000000, 0.09999999999999982514, 3.400000000000001243 ) ) ;
#1660 = DIRECTION ( 'NONE',  ( -0.000000000000000000, -1.000000000000000000, -0.000000000000000000 ) ) ;
#1661 = ORIENTED_EDGE ( 'NONE', *, *, #2538, .F. ) ;
#1662 = VERTEX_POINT ( 'NONE', #329 ) ;
#1663 = ORIENTED_EDGE ( 'NONE', *, *, #1875, .F. ) ;
#1664 = AXIS2_PLACEMENT_3D ( 'NONE', #2975, #7186, #11378 ) ;
#1665 = CARTESIAN_POINT ( 'NONE',  ( 54.70014691233865989, 3.000000000000000000, -3.785783530882224746 ) ) ;
#1666 = ORIENTED_EDGE ( 'NONE', *, *, #10488, .F. ) ;
#1667 = CARTESIAN_POINT ( 'NONE',  ( 2.453448243599948952, 0.000000000000000000, 2.353846153846153921 ) ) ;
#1668 = VERTEX_POINT ( 'NONE', #3475 ) ;
#1669 = CYLINDRICAL_SURFACE ( 'NONE', #1395, 1.500000000000000444 ) ;
#1670 = DIRECTION ( 'NONE',  ( 0.000000000000000000, 0.000000000000000000, 1.000000000000000000 ) ) ;
#1671 = DIRECTION ( 'NONE',  ( -0.7772490812546181127, 0.000000000000000000, -0.6291930273682727615 ) ) ;
#1672 = CARTESIAN_POINT ( 'NONE',  ( -5.975392301194336397, 0.000000000000000000, -6.045220165289885372 ) ) ;
#1673 =( GEOMETRIC_REPRESENTATION_CONTEXT ( 3 ) GLOBAL_UNCERTAINTY_ASSIGNED_CONTEXT ( ( #13299 ) ) GLOBAL_UNIT_ASSIGNED_CONTEXT ( ( #10404, #9299, #10607 ) ) REPRESENTATION_CONTEXT ( 'NONE', 'WORKASPACE' ) );
#1674 = DIRECTION ( 'NONE',  ( -2.312964634635743450E-15, -1.000000000000000000, 0.000000000000000000 ) ) ;
#1675 = CARTESIAN_POINT ( 'NONE',  ( 0.000000000000000000, 0.09999999999999982514, 0.000000000000000000 ) ) ;
#1676 = FACE_OUTER_BOUND ( 'NONE', #81, .T. ) ;
#1677 = ORIENTED_EDGE ( 'NONE', *, *, #9921, .T. ) ;
#1678 = FACE_OUTER_BOUND ( 'NONE', #5525, .T. ) ;
#1679 = ORIENTED_EDGE ( 'NONE', *, *, #5232, .T. ) ;
#1680 = ORIENTED_EDGE ( 'NONE', *, *, #6158, .F. ) ;
#1681 = CYLINDRICAL_SURFACE ( 'NONE', #6432, 8.499999999999998224 ) ;
#1682 = B_SPLINE_SURFACE_WITH_KNOTS ( 'NONE', 3, 1, ( 
 ( #1982, #5011 ),
 ( #948, #7285 ),
 ( #9206, #3968 ),
 ( #880, #11482 ) ),
 .UNSPECIFIED., .F., .F., .F.,
 ( 4, 4 ),
 ( 2, 2 ),
 ( 0.1547128134717859205, 1.000000000000000000 ),
 ( 0.000000000000000000, 1.000000000000000000 ),
 .UNSPECIFIED. ) ;
#1683 = ORIENTED_EDGE ( 'NONE', *, *, #770, .T. ) ;
#1684 = PRODUCT_DEFINITION_FORMATION_WITH_SPECIFIED_SOURCE ( 'ANY', '', #528, .NOT_KNOWN. ) ;
#1685 = ADVANCED_FACE ( 'NONE', ( #11623 ), #136, .T. ) ;
#1686 = DIRECTION ( 'NONE',  ( -0.000000000000000000, -1.000000000000000000, -0.000000000000000000 ) ) ;
#1687 = CARTESIAN_POINT ( 'NONE',  ( -8.158651161643904359, 3.000000000000000000, -8.922136023539605887 ) ) ;
#1688 = DIRECTION ( 'NONE',  ( 0.000000000000000000, 0.000000000000000000, 1.000000000000000000 ) ) ;
#1689 = CARTESIAN_POINT ( 'NONE',  ( -3.833392836528145331, 0.000000000000000000, -5.555861711818853799 ) ) ;
#1690 = CONTEXT_DEPENDENT_SHAPE_REPRESENTATION ( #1594, #12080 ) ;
#1691 = CARTESIAN_POINT ( 'NONE',  ( 0.4639228963249696913, 9.000000000000000000, 8.487330295579727846 ) ) ;
#1692 = CARTESIAN_POINT ( 'NONE',  ( -12.07793442604884682, 3.000000000000000000, 0.5400000000005513723 ) ) ;
#1693 = CARTESIAN_POINT ( 'NONE',  ( -3.893011711613112880, 3.000000000000000000, -12.40340517008282717 ) ) ;
#1694 = CARTESIAN_POINT ( 'NONE',  ( 3.469446951953614189E-15, 3.000000000000000000, -7.049999999999999822 ) ) ;
#1695 = DIRECTION ( 'NONE',  ( 0.000000000000000000, 1.000000000000000000, -0.000000000000000000 ) ) ;
#1696 = ORIENTED_EDGE ( 'NONE', *, *, #4159, .F. ) ;
#1697 = ORIENTED_EDGE ( 'NONE', *, *, #10199, .F. ) ;
#1698 = EDGE_CURVE ( 'NONE', #12325, #5342, #9679, .T. ) ;
#1699 = EDGE_LOOP ( 'NONE', ( #7649, #403, #11036, #4720 ) ) ;
#1700 = CARTESIAN_POINT ( 'NONE',  ( -21.21140389626389577, 3.000000000000000000, -14.83930531255815133 ) ) ;
#1701 = EDGE_CURVE ( 'NONE', #2851, #9443, #5618, .T. ) ;
#1702 = CARTESIAN_POINT ( 'NONE',  ( -6.970598036433426792, 0.000000000000000000, -10.97318381393771780 ) ) ;
#1703 = B_SPLINE_CURVE_WITH_KNOTS ( 'NONE', 3,
 ( #270, #7695, #7637, #2257 ),
 .UNSPECIFIED., .F., .F.,
 ( 4, 4 ),
 ( 0.1547128134717859205, 1.000000000000000000 ),
 .UNSPECIFIED. ) ;
#1704 = CARTESIAN_POINT ( 'NONE',  ( -8.430890348300632553, 3.000000000000000000, -11.48836750521723538 ) ) ;
#1705 = ADVANCED_FACE ( 'NONE', ( #8638 ), #3873, .F. ) ;
#1706 = FACE_OUTER_BOUND ( 'NONE', #9694, .T. ) ;
#1707 = CARTESIAN_POINT ( 'NONE',  ( -13.33579367773357482, 3.000000000000000000, 2.428572470324200427 ) ) ;
#1708 = CARTESIAN_POINT ( 'NONE',  ( 6.530577460941774603, 9.000000000000000000, 3.402183248810843885 ) ) ;
#1709 = DIRECTION ( 'NONE',  ( -0.000000000000000000, -1.000000000000000000, -0.000000000000000000 ) ) ;
#1710 = CARTESIAN_POINT ( 'NONE',  ( 8.158651161643900807, 0.000000000000000000, 8.922136023539609440 ) ) ;
#1711 = ORIENTED_EDGE ( 'NONE', *, *, #413, .T. ) ;
#1712 = B_SPLINE_SURFACE_WITH_KNOTS ( 'NONE', 3, 1, ( 
 ( #8387, #10606 ),
 ( #1097, #5174 ),
 ( #9497, #12614 ),
 ( #11581, #4338 ) ),
 .UNSPECIFIED., .F., .F., .F.,
 ( 4, 4 ),
 ( 2, 2 ),
 ( 0.1276832474596353850, 1.000000000000000000 ),
 ( 0.000000000000000000, 1.000000000000000000 ),
 .UNSPECIFIED. ) ;
#1713 = ORIENTED_EDGE ( 'NONE', *, *, #986, .F. ) ;
#1714 = VERTEX_POINT ( 'NONE', #4380 ) ;
#1715 = CARTESIAN_POINT ( 'NONE',  ( -2.546103534247749600, 0.000000000000000000, 12.55526518755974585 ) ) ;
#1716 = EDGE_CURVE ( 'NONE', #8003, #11262, #1524, .T. ) ;
#1717 = ORIENTED_EDGE ( 'NONE', *, *, #4452, .T. ) ;
#1718 = DIRECTION ( 'NONE',  ( -0.000000000000000000, -1.000000000000000000, -0.000000000000000000 ) ) ;
#1719 = DIRECTION ( 'NONE',  ( 0.9354619295301355164, -3.960764276234648707E-24, 0.3534274726160315794 ) ) ;
#1720 = EDGE_CURVE ( 'NONE', #11943, #175, #2501, .T. ) ;
#1721 = CARTESIAN_POINT ( 'NONE',  ( 4.690415759823430619, 2.900000000000000355, -1.500000000000000000 ) ) ;
#1722 = CARTESIAN_POINT ( 'NONE',  ( -14.90895795148411374, 3.000000000000000000, -1.650143266773683726 ) ) ;
#1723 = CARTESIAN_POINT ( 'NONE',  ( 12.00000000000001243, 4.999999999999999112, 10.00000000000000178 ) ) ;
#1724 = DIRECTION ( 'NONE',  ( 0.000000000000000000, 0.000000000000000000, -1.000000000000000000 ) ) ;
#1725 = CARTESIAN_POINT ( 'NONE',  ( 0.000000000000000000, 3.000000000000000000, 0.000000000000000000 ) ) ;
#1726 = ORIENTED_EDGE ( 'NONE', *, *, #7893, .F. ) ;
#1727 = CARTESIAN_POINT ( 'NONE',  ( -5.571433138827826426, 0.000000000000000000, -10.72973591378220526 ) ) ;
#1728 = VERTEX_POINT ( 'NONE', #4320 ) ;
#1729 = UNCERTAINTY_MEASURE_WITH_UNIT (LENGTH_MEASURE( 1.000000000000000082E-05 ), #103, 'distance_accuracy_value', 'NONE');
#1730 = ORIENTED_EDGE ( 'NONE', *, *, #5620, .T. ) ;
#1731 = CARTESIAN_POINT ( 'NONE',  ( 6.025412986832064277, 3.000000000000000000, -13.73660796332615597 ) ) ;
#1732 = ADVANCED_FACE ( 'NONE', ( #9746 ), #6375, .F. ) ;
#1733 = EDGE_CURVE ( 'NONE', #8766, #12346, #10724, .T. ) ;
#1734 = VERTEX_POINT ( 'NONE', #194 ) ;
#1735 = CARTESIAN_POINT ( 'NONE',  ( -10.69794375946289655, 3.000000000000000000, -7.065816209474156118 ) ) ;
#1736 = VERTEX_POINT ( 'NONE', #3413 ) ;
#1737 = CARTESIAN_POINT ( 'NONE',  ( -8.922226997226788470, 3.000000000000000000, -8.158551673544387484 ) ) ;
#1738 = FACE_OUTER_BOUND ( 'NONE', #5719, .T. ) ;
#1739 = DIRECTION ( 'NONE',  ( 0.000000000000000000, 1.000000000000000000, -0.000000000000000000 ) ) ;
#1740 = CARTESIAN_POINT ( 'NONE',  ( 12.00000000000001421, 6.000000000000000000, -3.122502256758250009E-15 ) ) ;
#1741 = CARTESIAN_POINT ( 'NONE',  ( -12.40340517008309185, 3.000000000000000000, -3.893011711613028947 ) ) ;
#1742 = VERTEX_POINT ( 'NONE', #5543 ) ;
#1743 = DIRECTION ( 'NONE',  ( 0.000000000000000000, 0.000000000000000000, -1.000000000000000000 ) ) ;
#1744 = ORIENTED_EDGE ( 'NONE', *, *, #11206, .T. ) ;
#1745 = ORIENTED_EDGE ( 'NONE', *, *, #9649, .F. ) ;
#1746 = DIRECTION ( 'NONE',  ( -0.000000000000000000, -1.000000000000000000, -0.000000000000000000 ) ) ;
#1747 = EDGE_CURVE ( 'NONE', #2399, #7044, #7623, .T. ) ;
#1748 = ORIENTED_EDGE ( 'NONE', *, *, #9633, .T. ) ;
#1749 = CARTESIAN_POINT ( 'NONE',  ( -6.025412986832177076, 3.000000000000000000, -13.73660796332610268 ) ) ;
#1750 = CARTESIAN_POINT ( 'NONE',  ( -5.039625798601655937, 0.000000000000000000, 4.490509081392509927 ) ) ;
#1751 = CARTESIAN_POINT ( 'NONE',  ( -7.494008246337227952, 0.000000000000000000, -11.63517940784355886 ) ) ;
#1752 = CARTESIAN_POINT ( 'NONE',  ( 11.99999999999999112, -4.572512030783488065E-14, -10.00000000000000178 ) ) ;
#1753 = CARTESIAN_POINT ( 'NONE',  ( 0.5400000000008001733, 3.000000000000000000, 12.07793442604883616 ) ) ;
#1754 = CONTEXT_DEPENDENT_SHAPE_REPRESENTATION ( #11191, #10521 ) ;
#1755 = DIRECTION ( 'NONE',  ( 0.000000000000000000, 0.000000000000000000, 1.000000000000000000 ) ) ;
#1756 = CARTESIAN_POINT ( 'NONE',  ( -8.430890348300632553, 3.000000000000000000, -11.48836750521723538 ) ) ;
#1757 = CARTESIAN_POINT ( 'NONE',  ( -3.647599401157625376, 0.000000000000000000, -11.52662650599085836 ) ) ;
#1758 = CARTESIAN_POINT ( 'NONE',  ( 31.00000000000000000, 3.000000000000000000, 0.000000000000000000 ) ) ;
#1759 = CARTESIAN_POINT ( 'NONE',  ( 2.525608486058770641, 2.900000000000000355, -2.423076923076923350 ) ) ;
#1760 = EDGE_LOOP ( 'NONE', ( #6272, #5206, #5825, #4814 ) ) ;
#1761 = ORIENTED_EDGE ( 'NONE', *, *, #4678, .F. ) ;
#1762 = ORIENTED_EDGE ( 'NONE', *, *, #13322, .F. ) ;
#1763 = ORIENTED_EDGE ( 'NONE', *, *, #5633, .F. ) ;
#1764 = CARTESIAN_POINT ( 'NONE',  ( 11.46814821560793618, 0.000000000000000000, -5.731782959214992701 ) ) ;
#1765 = DIRECTION ( 'NONE',  ( -0.000000000000000000, -1.000000000000000000, -0.000000000000000000 ) ) ;
#1766 = CARTESIAN_POINT ( 'NONE',  ( 4.690415759823430619, 0.09999999999999982514, 4.500000000000000888 ) ) ;
#1767 = CIRCLE ( 'NONE', #7482, 12.08999999999737440 ) ;
#1768 = CARTESIAN_POINT ( 'NONE',  ( 0.000000000000000000, 9.000000000000000000, 0.000000000000000000 ) ) ;
#1769 = CARTESIAN_POINT ( 'NONE',  ( 6.343080161942737938, 0.000000000000000000, -11.35348358516942469 ) ) ;
#1770 = VECTOR ( 'NONE', #4286, 1000.000000000000000 ) ;
#1771 = CARTESIAN_POINT ( 'NONE',  ( -14.82803603298498629, 3.000000000000000000, 2.264806262023049577 ) ) ;
#1772 = ADVANCED_FACE ( 'NONE', ( #5348 ), #4522, .F. ) ;
#1773 = EDGE_CURVE ( 'NONE', #3986, #6650, #1281, .T. ) ;
#1774 = CARTESIAN_POINT ( 'NONE',  ( 11.46814821560793618, 3.000000000000000000, -5.731782959214992701 ) ) ;
#1775 = ORIENTED_EDGE ( 'NONE', *, *, #5333, .F. ) ;
#1776 = EDGE_LOOP ( 'NONE', ( #8565, #9760, #5526, #11107 ) ) ;
#1777 = ORIENTED_EDGE ( 'NONE', *, *, #9452, .F. ) ;
#1778 = CARTESIAN_POINT ( 'NONE',  ( 1.650143266773734796, 0.000000000000000000, -14.90895795148410841 ) ) ;
#1779 = VECTOR ( 'NONE', #13132, 1000.000000000000000 ) ;
#1780 = CIRCLE ( 'NONE', #9471, 1.000000000000000888 ) ;
#1781 = ORIENTED_EDGE ( 'NONE', *, *, #2886, .F. ) ;
#1782 = CARTESIAN_POINT ( 'NONE',  ( -6.721397655168936502, 0.000000000000000000, 5.203154193476255074 ) ) ;
#1783 = DIRECTION ( 'NONE',  ( -0.5644961850934520076, 4.776414858632147300E-27, 0.8254356770911585039 ) ) ;
#1784 = DIRECTION ( 'NONE',  ( -0.000000000000000000, -1.000000000000000000, -0.000000000000000000 ) ) ;
#1785 = CARTESIAN_POINT ( 'NONE',  ( 26.30958424017656938, 0.09999999999999982514, 4.500000000000000888 ) ) ;
#1786 = CARTESIAN_POINT ( 'NONE',  ( -10.33484986938308303, 3.000000000000000000, 8.771102293099071190 ) ) ;
#1787 = VECTOR ( 'NONE', #5884, 1000.000000000000000 ) ;
#1788 = EDGE_CURVE ( 'NONE', #2335, #10776, #7481, .T. ) ;
#1789 = CARTESIAN_POINT ( 'NONE',  ( -4.564691384634503635, 0.000000000000000000, 12.76342233970727769 ) ) ;
#1790 = AXIS2_PLACEMENT_3D ( 'NONE', #7701, #11913, #2544 ) ;
#1791 = CARTESIAN_POINT ( 'NONE',  ( -0.8123631076467130452, 0.000000000000000000, -6.700937709107178009 ) ) ;
#1792 = ORIENTED_EDGE ( 'NONE', *, *, #969, .F. ) ;
#1793 = CARTESIAN_POINT ( 'NONE',  ( 0.000000000000000000, 3.000000000000000000, 0.000000000000000000 ) ) ;
#1794 = ORIENTED_EDGE ( 'NONE', *, *, #13063, .F. ) ;
#1795 = ORIENTED_EDGE ( 'NONE', *, *, #6353, .F. ) ;
#1796 = EDGE_CURVE ( 'NONE', #7728, #11178, #3583, .T. ) ;
#1797 = ORIENTED_EDGE ( 'NONE', *, *, #11017, .T. ) ;
#1798 = CARTESIAN_POINT ( 'NONE',  ( 3.000000000000001776, 0.000000000000000000, 10.00000000000000000 ) ) ;
#1799 = EDGE_CURVE ( 'NONE', #9584, #13244, #5679, .T. ) ;
#1800 = VERTEX_POINT ( 'NONE', #1633 ) ;
#1801 = LINE ( 'NONE', #11484, #10201 ) ;
#1802 = CIRCLE ( 'NONE', #253, 1.499999999999998668 ) ;
#1803 = ORIENTED_EDGE ( 'NONE', *, *, #11372, .F. ) ;
#1804 = CARTESIAN_POINT ( 'NONE',  ( 22.00000000000000000, 3.000000000000000000, -1.500000000000000666 ) ) ;
#1805 = CARTESIAN_POINT ( 'NONE',  ( 0.000000000000000000, 3.000000000000000000, 0.000000000000000000 ) ) ;
#1806 = FACE_OUTER_BOUND ( 'NONE', #13472, .T. ) ;
#1807 = CARTESIAN_POINT ( 'NONE',  ( -14.16466328168009881, 0.000000000000000000, 1.557181465540760534 ) ) ;
#1808 = CARTESIAN_POINT ( 'NONE',  ( 1.580708947611198623, 9.000000000000000000, -8.351727918397600092 ) ) ;
#1809 = LINE ( 'NONE', #6824, #4723 ) ;
#1810 = VERTEX_POINT ( 'NONE', #8771 ) ;
#1811 = AXIS2_PLACEMENT_3D ( 'NONE', #10518, #1077, #13417 ) ;
#1812 = CARTESIAN_POINT ( 'NONE',  ( -5.571313494980134173, 3.000000000000000000, 10.72979803820131295 ) ) ;
#1813 = AXIS2_PLACEMENT_3D ( 'NONE', #12705, #3315, #5319 ) ;
#1814 = VERTEX_POINT ( 'NONE', #1558 ) ;
#1815 = VERTEX_POINT ( 'NONE', #5826 ) ;
#1816 = CARTESIAN_POINT ( 'NONE',  ( -5.571433138827826426, 3.000000000000000000, -10.72973591378220526 ) ) ;
#1817 = ORIENTED_EDGE ( 'NONE', *, *, #11409, .F. ) ;
#1818 = CARTESIAN_POINT ( 'NONE',  ( 0.000000000000000000, 9.000000000000000000, 0.000000000000000000 ) ) ;
#1819 = VECTOR ( 'NONE', #9647, 1000.000000000000000 ) ;
#1820 = CARTESIAN_POINT ( 'NONE',  ( -11.80615107470192804, 3.000000000000000000, -2.604399508764160487 ) ) ;
#1821 = AXIS2_PLACEMENT_3D ( 'NONE', #903, #7240, #11235 ) ;
#1822 = VECTOR ( 'NONE', #2673, 1000.000000000000000 ) ;
#1823 = DIRECTION ( 'NONE',  ( 0.000000000000000000, 0.000000000000000000, 1.000000000000000000 ) ) ;
#1824 = DIRECTION ( 'NONE',  ( 0.000000000000000000, 0.000000000000000000, 1.000000000000000000 ) ) ;
#1825 = B_SPLINE_CURVE_WITH_KNOTS ( 'NONE', 3,
 ( #12649, #2229, #6436, #10647 ),
 .UNSPECIFIED., .F., .F.,
 ( 4, 4 ),
 ( 0.1276832474596353850, 1.000000000000000000 ),
 .UNSPECIFIED. ) ;
#1826 = DIRECTION ( 'NONE',  ( 0.000000000000000000, 1.000000000000000000, 0.000000000000000000 ) ) ;
#1827 = ITEM_DEFINED_TRANSFORMATION ( 'NONE', 'NONE', #4533,  #10007 ) ;
#1828 = CARTESIAN_POINT ( 'NONE',  ( 0.000000000000000000, 3.000000000000000000, 0.000000000000000000 ) ) ;
#1829 = EDGE_CURVE ( 'NONE', #5704, #11250, #10986, .T. ) ;
#1830 = CARTESIAN_POINT ( 'NONE',  ( -0.6724118135763151871, 3.000000000000000000, -13.82336506795071784 ) ) ;
#1831 = CARTESIAN_POINT ( 'NONE',  ( -13.49999999999999645, 3.000000000000000000, -7.049999999999998934 ) ) ;
#1832 = CYLINDRICAL_SURFACE ( 'NONE', #6028, 3.499999999999999556 ) ;
#1833 = CARTESIAN_POINT ( 'NONE',  ( -8.158651161643904359, 3.000000000000000000, -8.922136023539605887 ) ) ;
#1834 = ORIENTED_EDGE ( 'NONE', *, *, #10278, .T. ) ;
#1835 = CIRCLE ( 'NONE', #4026, 6.749999999999999112 ) ;
#1836 = ORIENTED_EDGE ( 'NONE', *, *, #303, .F. ) ;
#1837 = ORIENTED_EDGE ( 'NONE', *, *, #5832, .T. ) ;
#1838 = VERTEX_POINT ( 'NONE', #598 ) ;
#1839 = CARTESIAN_POINT ( 'NONE',  ( 8.158651161643900807, 0.000000000000000000, 8.922136023539609440 ) ) ;
#1840 = DIRECTION ( 'NONE',  ( 0.000000000000000000, 0.000000000000000000, -1.000000000000000000 ) ) ;
#1841 = CIRCLE ( 'NONE', #10407, 3.400000000000001243 ) ;
#1842 = CARTESIAN_POINT ( 'NONE',  ( -8.795158114916672432, 3.000000000000000000, -9.573149624528774382 ) ) ;
#1843 = AXIS2_PLACEMENT_3D ( 'NONE', #1828, #6775, #4714 ) ;
#1844 = DIRECTION ( 'NONE',  ( 0.000000000000000000, 0.000000000000000000, 1.000000000000000000 ) ) ;
#1845 = DIRECTION ( 'NONE',  ( 0.000000000000000000, 0.000000000000000000, 1.000000000000000000 ) ) ;
#1846 = CARTESIAN_POINT ( 'NONE',  ( -12.79759916868914615, 3.000000000000000000, -0.7702044561450367421 ) ) ;
#1847 = CARTESIAN_POINT ( 'NONE',  ( -0.7702044561450404059, 0.000000000000000000, 12.79759916868914793 ) ) ;
#1848 = ORIENTED_EDGE ( 'NONE', *, *, #5747, .F. ) ;
#1849 = CARTESIAN_POINT ( 'NONE',  ( 12.57851281883977457, 3.000000000000000000, 3.283445639306028063 ) ) ;
#1850 = VECTOR ( 'NONE', #1150, 1000.000000000000227 ) ;
#1851 = CARTESIAN_POINT ( 'NONE',  ( 4.201465772524378472, 9.000000000000000000, 6.047394330962382547 ) ) ;
#1852 = VECTOR ( 'NONE', #9576, 1000.000000000000000 ) ;
#1853 = EDGE_LOOP ( 'NONE', ( #6961, #4497, #1680, #7692 ) ) ;
#1854 = EDGE_CURVE ( 'NONE', #6430, #6340, #12989, .T. ) ;
#1855 = CARTESIAN_POINT ( 'NONE',  ( -2.161962830978785277, 0.000000000000000000, -14.08504230442586369 ) ) ;
#1856 = DIRECTION ( 'NONE',  ( 0.9354619295301355164, -3.960764276234648707E-24, 0.3534274726160315794 ) ) ;
#1857 = CARTESIAN_POINT ( 'NONE',  ( -3.533475733155565290, 9.000000000000000000, 7.730753471893975437 ) ) ;
#1858 = CARTESIAN_POINT ( 'NONE',  ( 7.712570079660896916, 3.000000000000000000, -11.14709020439929432 ) ) ;
#1859 = AXIS2_PLACEMENT_3D ( 'NONE', #3543, #10859, #2450 ) ;
#1860 = CARTESIAN_POINT ( 'NONE',  ( 4.690415759823430619, 2.900000000000000355, 1.399999999999999911 ) ) ;
#1861 = AXIS2_PLACEMENT_3D ( 'NONE', #5283, #260, #9485 ) ;
#1862 = LINE ( 'NONE', #7167, #5318 ) ;
#1863 = DIRECTION ( 'NONE',  ( -0.000000000000000000, -1.000000000000000000, -0.000000000000000000 ) ) ;
#1864 = VERTEX_POINT ( 'NONE', #9049 ) ;
#1865 = DIRECTION ( 'NONE',  ( 0.000000000000000000, 1.000000000000000000, -0.000000000000000000 ) ) ;
#1866 =( REPRESENTATION_RELATIONSHIP ('NONE','NONE', #3798, #8461 ) REPRESENTATION_RELATIONSHIP_WITH_TRANSFORMATION ( #12448 )SHAPE_REPRESENTATION_RELATIONSHIP( ) );
#1867 = ORIENTED_EDGE ( 'NONE', *, *, #432, .T. ) ;
#1868 = UNCERTAINTY_MEASURE_WITH_UNIT (LENGTH_MEASURE( 1.000000000000000082E-05 ), #9482, 'distance_accuracy_value', 'NONE');
#1869 = ORIENTED_EDGE ( 'NONE', *, *, #6836, .F. ) ;
#1870 = ORIENTED_EDGE ( 'NONE', *, *, #9876, .T. ) ;
#1871 = CARTESIAN_POINT ( 'NONE',  ( 8.430890348300586368, 0.000000000000000000, -11.48836750521726913 ) ) ;
#1872 = ORIENTED_EDGE ( 'NONE', *, *, #3526, .F. ) ;
#1873 = CIRCLE ( 'NONE', #7153, 6.750000000000000888 ) ;
#1874 = VECTOR ( 'NONE', #12257, 1000.000000000000000 ) ;
#1875 = EDGE_CURVE ( 'NONE', #9276, #10087, #11385, .T. ) ;
#1876 = CARTESIAN_POINT ( 'NONE',  ( 3.555260608155775159, 9.000000000000000000, 7.720759160088846329 ) ) ;
#1877 = SURFACE_SIDE_STYLE ('',( #11233 ) ) ;
#1878 = CARTESIAN_POINT ( 'NONE',  ( 26.30958424017656938, 3.000000000000000000, -4.500000000000000888 ) ) ;
#1879 = EDGE_CURVE ( 'NONE', #2097, #9662, #3747, .T. ) ;
#1880 = DIRECTION ( 'NONE',  ( -1.000000000000000000, -0.000000000000000000, -0.000000000000000000 ) ) ;
#1881 = ADVANCED_FACE ( 'NONE', ( #10159 ), #10089, .T. ) ;
#1882 = CARTESIAN_POINT ( 'NONE',  ( 3.555260608155774271, 0.000000000000000000, 7.720759160088842776 ) ) ;
#1883 = DIRECTION ( 'NONE',  ( -0.000000000000000000, -1.000000000000000000, -0.000000000000000000 ) ) ;
#1884 = ORIENTED_EDGE ( 'NONE', *, *, #8272, .T. ) ;
#1885 = DIRECTION ( 'NONE',  ( 0.000000000000000000, 0.000000000000000000, 1.000000000000000000 ) ) ;
#1886 = VECTOR ( 'NONE', #961, 1000.000000000000000 ) ;
#1887 = VERTEX_POINT ( 'NONE', #7952 ) ;
#1888 = EDGE_LOOP ( 'NONE', ( #6480, #9877 ) ) ;
#1889 = CARTESIAN_POINT ( 'NONE',  ( -4.340891659662447388, -1.694065894508600678E-18, 6.651128039276029469 ) ) ;
#1890 = ORIENTED_EDGE ( 'NONE', *, *, #10284, .T. ) ;
#1891 = ADVANCED_FACE ( 'NONE', ( #12099 ), #351, .F. ) ;
#1892 = CARTESIAN_POINT ( 'NONE',  ( -6.558450276537426404, 9.000000000000000000, -1.596630818375423866 ) ) ;
#1893 = AXIS2_PLACEMENT_3D ( 'NONE', #8934, #3975, #5770 ) ;
#1894 = AXIS2_PLACEMENT_3D ( 'NONE', #10392, #13498, #1 ) ;
#1895 = CARTESIAN_POINT ( 'NONE',  ( 10.98198414889934682, 3.000000000000000000, -9.379342464487748998 ) ) ;
#1896 = CARTESIAN_POINT ( 'NONE',  ( 13.04554897075798081, 0.000000000000000000, -5.733772933379503556 ) ) ;
#1897 = DIRECTION ( 'NONE',  ( 1.000000000000000000, -0.000000000000000000, 0.000000000000000000 ) ) ;
#1898 = CARTESIAN_POINT ( 'NONE',  ( -5.784789447945489549, 0.000000000000000000, 12.25836857253663581 ) ) ;
#1899 = DIRECTION ( 'NONE',  ( 1.000000000000000000, -3.491481338843133355E-15, -2.602085213965210149E-16 ) ) ;
#1900 = B_SPLINE_SURFACE_WITH_KNOTS ( 'NONE', 3, 1, ( 
 ( #5211, #9268 ),
 ( #874, #9548 ),
 ( #6073, #8362 ),
 ( #8162, #12392 ) ),
 .UNSPECIFIED., .F., .F., .F.,
 ( 4, 4 ),
 ( 2, 2 ),
 ( 0.000000000000000000, 0.8452273900860258760 ),
 ( 0.000000000000000000, 1.000000000000000000 ),
 .UNSPECIFIED. ) ;
#1901 = EDGE_CURVE ( 'NONE', #6718, #12346, #8914, .T. ) ;
#1902 = FACE_OUTER_BOUND ( 'NONE', #353, .T. ) ;
#1903 = DIRECTION ( 'NONE',  ( -0.000000000000000000, -1.000000000000000000, -0.000000000000000000 ) ) ;
#1904 = DIRECTION ( 'NONE',  ( -0.000000000000000000, -1.000000000000000000, -0.000000000000000000 ) ) ;
#1905 = CARTESIAN_POINT ( 'NONE',  ( 10.72973591378220704, 3.000000000000000000, -5.571433138827823761 ) ) ;
#1906 = ORIENTED_EDGE ( 'NONE', *, *, #3581, .T. ) ;
#1907 = PRODUCT_DEFINITION_FORMATION_WITH_SPECIFIED_SOURCE ( 'ANY', '', #7531, .NOT_KNOWN. ) ;
#1908 = ORIENTED_EDGE ( 'NONE', *, *, #8249, .T. ) ;
#1909 = EDGE_LOOP ( 'NONE', ( #12844, #5302, #9727, #3674 ) ) ;
#1910 = EDGE_CURVE ( 'NONE', #1668, #1714, #12249, .T. ) ;
#1911 = ADVANCED_FACE ( 'NONE', ( #7749 ), #10138, .F. ) ;
#1912 = ORIENTED_EDGE ( 'NONE', *, *, #6042, .F. ) ;
#1913 = DIRECTION ( 'NONE',  ( -0.000000000000000000, -1.000000000000000000, -0.000000000000000000 ) ) ;
#1914 = DIRECTION ( 'NONE',  ( 0.7216024245882217691, 0.000000000000000000, -0.6923076923076904032 ) ) ;
#1915 = B_SPLINE_SURFACE_WITH_KNOTS ( 'NONE', 3, 1, ( 
 ( #3445, #568 ),
 ( #13165, #2685 ),
 ( #6890, #7654 ),
 ( #11857, #2416 ) ),
 .UNSPECIFIED., .F., .F., .F.,
 ( 4, 4 ),
 ( 2, 2 ),
 ( 0.000000000000000000, 0.5855695330273008592 ),
 ( 0.000000000000000000, 1.000000000000000000 ),
 .UNSPECIFIED. ) ;
#1916 = CARTESIAN_POINT ( 'NONE',  ( -14.87484884897975057, 3.000000000000000000, 1.958311002203303453 ) ) ;
#1917 = DIRECTION ( 'NONE',  ( 0.000000000000000000, 1.000000000000000000, 0.000000000000000000 ) ) ;
#1918 = CYLINDRICAL_SURFACE ( 'NONE', #5087, 1.000000000000000888 ) ;
#1919 = CARTESIAN_POINT ( 'NONE',  ( -13.28140389626389783, 0.000000000000000000, 13.39999999999999858 ) ) ;
#1920 = CARTESIAN_POINT ( 'NONE',  ( 0.000000000000000000, 0.000000000000000000, 0.000000000000000000 ) ) ;
#1921 = ORIENTED_EDGE ( 'NONE', *, *, #9861, .T. ) ;
#1922 = FACE_OUTER_BOUND ( 'NONE', #3038, .T. ) ;
#1923 = CARTESIAN_POINT ( 'NONE',  ( -3.188443695493920593, 0.000000000000000000, -12.60833606734848189 ) ) ;
#1924 = VERTEX_POINT ( 'NONE', #1488 ) ;
#1925 = CARTESIAN_POINT ( 'NONE',  ( 8.922136023539611216, 0.000000000000000000, -8.158651161643899030 ) ) ;
#1926 = DIRECTION ( 'NONE',  ( -0.000000000000000000, -1.000000000000000000, -0.000000000000000000 ) ) ;
#1927 = CARTESIAN_POINT ( 'NONE',  ( -12.16218796965919324, 0.000000000000000000, -4.056222772158363021 ) ) ;
#1928 = DIRECTION ( 'NONE',  ( -0.000000000000000000, -1.000000000000000000, -0.000000000000000000 ) ) ;
#1929 = CARTESIAN_POINT ( 'NONE',  ( -12.60833596047604210, 0.000000000000000000, -3.188441730140805674 ) ) ;
#1930 = DIRECTION ( 'NONE',  ( 0.000000000000000000, 1.000000000000000000, 0.000000000000000000 ) ) ;
#1931 = ORIENTED_EDGE ( 'NONE', *, *, #3127, .T. ) ;
#1932 = EDGE_CURVE ( 'NONE', #6498, #3264, #2934, .T. ) ;
#1933 = VERTEX_POINT ( 'NONE', #8838 ) ;
#1934 = ORIENTED_EDGE ( 'NONE', *, *, #3335, .T. ) ;
#1935 = CARTESIAN_POINT ( 'NONE',  ( 0.000000000000000000, 3.000000000000000000, 0.000000000000000000 ) ) ;
#1936 = ORIENTED_EDGE ( 'NONE', *, *, #3341, .F. ) ;
#1937 = CARTESIAN_POINT ( 'NONE',  ( 0.000000000000000000, 0.000000000000000000, 0.000000000000000000 ) ) ;
#1938 = FILL_AREA_STYLE_COLOUR ( '', #13317 ) ;
#1939 = FACE_OUTER_BOUND ( 'NONE', #12013, .T. ) ;
#1940 = CARTESIAN_POINT ( 'NONE',  ( 0.7868956173019259204, 0.000000000000000000, 7.903520140620750034 ) ) ;
#1941 = CARTESIAN_POINT ( 'NONE',  ( 1.650143266773734796, 0.000000000000000000, -14.90895795148410841 ) ) ;
#1942 = DIRECTION ( 'NONE',  ( -0.000000000000000000, -1.000000000000000000, -0.000000000000000000 ) ) ;
#1943 = CARTESIAN_POINT ( 'NONE',  ( 11.11702303352194043, 0.000000000000000000, -8.914835885878249044 ) ) ;
#1944 = ORIENTED_EDGE ( 'NONE', *, *, #2600, .F. ) ;
#1945 = DIRECTION ( 'NONE',  ( -0.000000000000000000, -1.000000000000000000, -0.000000000000000000 ) ) ;
#1946 = ADVANCED_FACE ( 'NONE', ( #13059 ), #3617, .T. ) ;
#1947 = ORIENTED_EDGE ( 'NONE', *, *, #12833, .T. ) ;
#1948 = EDGE_CURVE ( 'NONE', #3825, #916, #12465, .T. ) ;
#1949 = EDGE_LOOP ( 'NONE', ( #12098, #12630, #4544, #1473 ) ) ;
#1950 = CARTESIAN_POINT ( 'NONE',  ( 11.99999999999999467, -5.150753189442425446E-14, 10.00000000000000000 ) ) ;
#1951 = ORIENTED_EDGE ( 'NONE', *, *, #8465, .F. ) ;
#1952 = EDGE_CURVE ( 'NONE', #12534, #13401, #6453, .T. ) ;
#1953 = DIRECTION ( 'NONE',  ( 0.000000000000000000, 0.000000000000000000, 1.000000000000000000 ) ) ;
#1954 =( LENGTH_UNIT ( ) NAMED_UNIT ( * ) SI_UNIT ( .MILLI., .METRE. ) );
#1955 = CARTESIAN_POINT ( 'NONE',  ( -12.56087513340552242, 3.000000000000000000, 2.568302020731519253 ) ) ;
#1956 = CARTESIAN_POINT ( 'NONE',  ( 26.30958424017656938, 3.000000000000000000, 1.399999999999999911 ) ) ;
#1957 = DIRECTION ( 'NONE',  ( -0.000000000000000000, -1.000000000000000000, -0.000000000000000000 ) ) ;
#1958 = LINE ( 'NONE', #13534, #11523 ) ;
#1959 = CARTESIAN_POINT ( 'NONE',  ( -8.100301009650799244, 0.000000000000000000, -2.575873357339268033 ) ) ;
#1960 = CARTESIAN_POINT ( 'NONE',  ( -4.334442004268525217, 0.000000000000000000, 7.311813216407587745 ) ) ;
#1961 = CARTESIAN_POINT ( 'NONE',  ( -14.90895795148409420, 3.000000000000000000, 1.650143266773909101 ) ) ;
#1962 = ORIENTED_EDGE ( 'NONE', *, *, #388, .T. ) ;
#1963 = CARTESIAN_POINT ( 'NONE',  ( 0.000000000000000000, 3.000000000000000000, 0.000000000000000000 ) ) ;
#1964 = EDGE_CURVE ( 'NONE', #5535, #13368, #9406, .T. ) ;
#1965 = ORIENTED_EDGE ( 'NONE', *, *, #9188, .F. ) ;
#1966 = CIRCLE ( 'NONE', #3700, 3.399999999999999911 ) ;
#1967 = ORIENTED_EDGE ( 'NONE', *, *, #8053, .T. ) ;
#1968 = VERTEX_POINT ( 'NONE', #6164 ) ;
#1969 = EDGE_CURVE ( 'NONE', #8365, #12893, #8158, .T. ) ;
#1970 = EDGE_CURVE ( 'NONE', #3576, #11919, #6278, .T. ) ;
#1971 = EDGE_LOOP ( 'NONE', ( #10807, #2206, #785, #12247 ) ) ;
#1972 = CARTESIAN_POINT ( 'NONE',  ( -3.188443695493920593, 3.000000000000000000, -12.60833606734848189 ) ) ;
#1973 = CARTESIAN_POINT ( 'NONE',  ( 55.44259468463320673, 3.000000000000000000, -4.702937446762657459 ) ) ;
#1974 = DIRECTION ( 'NONE',  ( -0.000000000000000000, -1.000000000000000000, -0.000000000000000000 ) ) ;
#1975 = LINE ( 'NONE', #1012, #7945 ) ;
#1976 = CARTESIAN_POINT ( 'NONE',  ( -8.430890348300124515, 3.000000000000000000, 11.48836750521761019 ) ) ;
#1977 = VECTOR ( 'NONE', #1151, 1000.000000000000000 ) ;
#1978 = DIRECTION ( 'NONE',  ( -0.000000000000000000, -1.000000000000000000, -0.000000000000000000 ) ) ;
#1979 = CARTESIAN_POINT ( 'NONE',  ( -1.557181465540677712, 0.000000000000000000, 14.16466328168010769 ) ) ;
#1980 = ORIENTED_EDGE ( 'NONE', *, *, #13096, .F. ) ;
#1981 = DIRECTION ( 'NONE',  ( 0.000000000000000000, 0.000000000000000000, 1.000000000000000000 ) ) ;
#1982 = CARTESIAN_POINT ( 'NONE',  ( 10.72979803820132005, 3.000000000000000000, 5.571313494980133285 ) ) ;
#1983 = ORIENTED_EDGE ( 'NONE', *, *, #5070, .F. ) ;
#1984 = AXIS2_PLACEMENT_3D ( 'NONE', #12867, #3620, #9956 ) ;
#1985 = AXIS2_PLACEMENT_3D ( 'NONE', #7485, #13560, #7289 ) ;
#1986 = DIRECTION ( 'NONE',  ( 0.000000000000000000, 1.000000000000000000, 0.000000000000000000 ) ) ;
#1987 = APPLICATION_PROTOCOL_DEFINITION ( 'draft international standard', 'automotive_design', 1998, #4935 ) ;
#1988 = CARTESIAN_POINT ( 'NONE',  ( 0.7702044561450380744, 3.000000000000000000, -12.79759916868914615 ) ) ;
#1989 = DIRECTION ( 'NONE',  ( -0.000000000000000000, -1.000000000000000000, -0.000000000000000000 ) ) ;
#1990 = DIRECTION ( 'NONE',  ( 0.000000000000000000, 0.000000000000000000, 1.000000000000000000 ) ) ;
#1991 = EDGE_CURVE ( 'NONE', #781, #2012, #11343, .T. ) ;
#1992 = CARTESIAN_POINT ( 'NONE',  ( 30.73000000000000043, 3.000000000000000000, -2.499999999999995115 ) ) ;
#1993 = EDGE_CURVE ( 'NONE', #12500, #12757, #7554, .T. ) ;
#1994 = CARTESIAN_POINT ( 'NONE',  ( 2.720000000000001528, 0.000000000000000000, 7.500000000000000888 ) ) ;
#1995 = VECTOR ( 'NONE', #12447, 1000.000000000000000 ) ;
#1996 = ORIENTED_EDGE ( 'NONE', *, *, #12521, .F. ) ;
#1997 = AXIS2_PLACEMENT_3D ( 'NONE', #12007, #8886, #3511 ) ;
#1998 = VERTEX_POINT ( 'NONE', #4031 ) ;
#1999 = CYLINDRICAL_SURFACE ( 'NONE', #9067, 14.25000000000000000 ) ;
#2000 = ORIENTED_EDGE ( 'NONE', *, *, #2363, .T. ) ;
#2001 = CYLINDRICAL_SURFACE ( 'NONE', #418, 3.999999999999997335 ) ;
#2002 = VECTOR ( 'NONE', #2219, 1000.000000000000000 ) ;
#2003 = CARTESIAN_POINT ( 'NONE',  ( -6.506507307819711095, 0.000000000000000000, 10.18987059060247624 ) ) ;
#2004 = DIRECTION ( 'NONE',  ( 0.6923076923076927347, 3.129451665637426527E-15, 0.7216024245882196597 ) ) ;
#2005 = CIRCLE ( 'NONE', #10360, 5.486375544325371223 ) ;
#2006 = B_SPLINE_CURVE_WITH_KNOTS ( 'NONE', 3,
 ( #9525, #172, #106, #4288 ),
 .UNSPECIFIED., .F., .F.,
 ( 4, 4 ),
 ( 0.1547128134717859205, 0.7774895956119340923 ),
 .UNSPECIFIED. ) ;
#2007 = FACE_OUTER_BOUND ( 'NONE', #1504, .T. ) ;
#2008 = LINE ( 'NONE', #6202, #3327 ) ;
#2009 = LINE ( 'NONE', #6271, #5183 ) ;
#2010 = ORIENTED_EDGE ( 'NONE', *, *, #7467, .F. ) ;
#2011 = CARTESIAN_POINT ( 'NONE',  ( 2.394769219159762930, 1.734723475976807094E-15, -6.310909632292713844 ) ) ;
#2012 = VERTEX_POINT ( 'NONE', #3003 ) ;
#2013 = VERTEX_POINT ( 'NONE', #11469 ) ;
#2014 = CARTESIAN_POINT ( 'NONE',  ( -5.741477348071430065, 0.000000000000000000, -13.86115248177175374 ) ) ;
#2015 = AXIS2_PLACEMENT_3D ( 'NONE', #6511, #10715, #5464 ) ;
#2016 = AXIS2_PLACEMENT_3D ( 'NONE', #3607, #2438, #8760 ) ;
#2017 = ORIENTED_EDGE ( 'NONE', *, *, #12673, .F. ) ;
#2018 = CARTESIAN_POINT ( 'NONE',  ( 0.000000000000000000, 0.09999999999999982514, 0.000000000000000000 ) ) ;
#2019 = DIRECTION ( 'NONE',  ( 0.000000000000000000, 0.000000000000000000, 1.000000000000000000 ) ) ;
#2020 = CARTESIAN_POINT ( 'NONE',  ( -10.97318381393799136, 0.000000000000000000, -6.970598036433411693 ) ) ;
#2021 = DIRECTION ( 'NONE',  ( 0.000000000000000000, 1.000000000000000000, 0.000000000000000000 ) ) ;
#2022 = EDGE_CURVE ( 'NONE', #4834, #8240, #9329, .T. ) ;
#2023 = CARTESIAN_POINT ( 'NONE',  ( -2.411622991978541464, 9.000000000000000000, -6.304488444319688689 ) ) ;
#2024 = ITEM_DEFINED_TRANSFORMATION ( 'NONE', 'NONE', #10908,  #10007 ) ;
#2025 = DIRECTION ( 'NONE',  ( -0.000000000000000000, -1.000000000000000000, -0.000000000000000000 ) ) ;
#2026 = AXIS2_PLACEMENT_3D ( 'NONE', #8392, #1373, #7643 ) ;
#2027 = CARTESIAN_POINT ( 'NONE',  ( -14.08504230442586369, 3.000000000000000000, 2.161962830978781724 ) ) ;
#2028 = DIRECTION ( 'NONE',  ( -1.000000000000000000, 3.469446951953610639E-15, 2.602085213965210149E-16 ) ) ;
#2029 = VERTEX_POINT ( 'NONE', #13547 ) ;
#2030 = DIRECTION ( 'NONE',  ( -0.000000000000000000, -1.000000000000000000, -0.000000000000000000 ) ) ;
#2031 = ORIENTED_EDGE ( 'NONE', *, *, #8422, .F. ) ;
#2032 = ORIENTED_EDGE ( 'NONE', *, *, #11788, .F. ) ;
#2033 = VERTEX_POINT ( 'NONE', #12583 ) ;
#2034 = AXIS2_PLACEMENT_3D ( 'NONE', #3071, #7284, #11481 ) ;
#2035 = VECTOR ( 'NONE', #4236, 1000.000000000000000 ) ;
#2036 = EDGE_LOOP ( 'NONE', ( #416, #5647, #158, #8553 ) ) ;
#2037 = LINE ( 'NONE', #1009, #527 ) ;
#2038 = DIRECTION ( 'NONE',  ( 0.000000000000000000, 0.000000000000000000, -1.000000000000000000 ) ) ;
#2039 = ADVANCED_FACE ( 'NONE', ( #2857 ), #6234, .F. ) ;
#2040 = FACE_OUTER_BOUND ( 'NONE', #3559, .T. ) ;
#2041 = APPLICATION_CONTEXT ( 'automotive_design' ) ;
#2042 = CARTESIAN_POINT ( 'NONE',  ( 0.7702044561450380744, 3.000000000000000000, -12.79759916868914615 ) ) ;
#2043 = CARTESIAN_POINT ( 'NONE',  ( 6.970598036433451661, 0.000000000000000000, -10.97318381393796294 ) ) ;
#2044 = AXIS2_PLACEMENT_3D ( 'NONE', #9984, #4819, #8061 ) ;
#2045 = EDGE_CURVE ( 'NONE', #4765, #7515, #2995, .T. ) ;
#2046 = AXIS2_PLACEMENT_3D ( 'NONE', #3810, #13115, #585 ) ;
#2047 = EDGE_CURVE ( 'NONE', #5599, #2682, #12427, .T. ) ;
#2048 = ORIENTED_EDGE ( 'NONE', *, *, #108, .T. ) ;
#2049 = CARTESIAN_POINT ( 'NONE',  ( -7.144272221052618832, 0.000000000000000000, 1.784003156764502940 ) ) ;
#2050 = CARTESIAN_POINT ( 'NONE',  ( 0.000000000000000000, 14.00000000000000178, 0.000000000000000000 ) ) ;
#2051 = ORIENTED_EDGE ( 'NONE', *, *, #3303, .F. ) ;
#2052 = CARTESIAN_POINT ( 'NONE',  ( 24.82664254338761722, 3.000000000000000000, 4.561072489069574409 ) ) ;
#2053 = AXIS2_PLACEMENT_3D ( 'NONE', #13357, #4804, #5841 ) ;
#2054 = EDGE_CURVE ( 'NONE', #13453, #2354, #11308, .T. ) ;
#2055 = DIRECTION ( 'NONE',  ( -0.000000000000000000, -1.000000000000000000, 0.000000000000000000 ) ) ;
#2056 = SHAPE_DEFINITION_REPRESENTATION ( #6336, #8376 ) ;
#2057 = LINE ( 'NONE', #8572, #5961 ) ;
#2058 = DIRECTION ( 'NONE',  ( -0.000000000000000000, -1.000000000000000000, -0.000000000000000000 ) ) ;
#2059 = CARTESIAN_POINT ( 'NONE',  ( -9.593885948927676210, 3.000000000000000000, 8.504652361247165615 ) ) ;
#2060 = EDGE_CURVE ( 'NONE', #930, #13159, #3377, .T. ) ;
#2061 = DIRECTION ( 'NONE',  ( -0.000000000000000000, -1.000000000000000000, -0.000000000000000000 ) ) ;
#2062 = VECTOR ( 'NONE', #7421, 1000.000000000000000 ) ;
#2063 = CARTESIAN_POINT ( 'NONE',  ( 0.000000000000000000, 3.000000000000000000, 0.000000000000000000 ) ) ;
#2064 = AXIS2_PLACEMENT_3D ( 'NONE', #4291, #11862, #3386 ) ;
#2065 = TOROIDAL_SURFACE ( 'NONE', #5140, 3.399999999999999911, 0.1000000000000000056 ) ;
#2066 = VERTEX_POINT ( 'NONE', #5134 ) ;
#2067 = ORIENTED_EDGE ( 'NONE', *, *, #3148, .F. ) ;
#2068 = VERTEX_POINT ( 'NONE', #2105 ) ;
#2069 = CARTESIAN_POINT ( 'NONE',  ( -0.1834773636644435324, 0.000000000000000000, -13.00394737445024873 ) ) ;
#2070 = ORIENTED_EDGE ( 'NONE', *, *, #4899, .T. ) ;
#2071 = EDGE_CURVE ( 'NONE', #10341, #8124, #2037, .T. ) ;
#2072 = EDGE_CURVE ( 'NONE', #5132, #3799, #6297, .T. ) ;
#2073 = FACE_BOUND ( 'NONE', #18, .T. ) ;
#2074 = AXIS2_PLACEMENT_3D ( 'NONE', #10610, #10742, #9502 ) ;
#2075 = CARTESIAN_POINT ( 'NONE',  ( 5.733772933379474246, 0.000000000000000000, -13.04554897075799502 ) ) ;
#2076 = VECTOR ( 'NONE', #10909, 1000.000000000000000 ) ;
#2077 = CARTESIAN_POINT ( 'NONE',  ( 0.000000000000000000, 3.000000000000000000, 0.000000000000000000 ) ) ;
#2078 = CARTESIAN_POINT ( 'NONE',  ( -12.56843238770841786, 3.000000000000000000, 3.367671042046304741 ) ) ;
#2079 = CARTESIAN_POINT ( 'NONE',  ( 1.650143266773734796, 3.000000000000000000, -14.90895795148410841 ) ) ;
#2080 = ORIENTED_EDGE ( 'NONE', *, *, #1964, .F. ) ;
#2081 = CARTESIAN_POINT ( 'NONE',  ( -2.481593227817850966, 0.000000000000000000, -8.129679886173169834 ) ) ;
#2082 = VERTEX_POINT ( 'NONE', #11267 ) ;
#2083 = VERTEX_POINT ( 'NONE', #1839 ) ;
#2084 = CIRCLE ( 'NONE', #1645, 14.25000000000000178 ) ;
#2085 = DIRECTION ( 'NONE',  ( 0.000000000000000000, 0.000000000000000000, -1.000000000000000000 ) ) ;
#2086 = EDGE_LOOP ( 'NONE', ( #3854, #8076 ) ) ;
#2087 = CARTESIAN_POINT ( 'NONE',  ( 0.000000000000000000, 0.000000000000000000, 0.000000000000000000 ) ) ;
#2088 = DIRECTION ( 'NONE',  ( 0.000000000000000000, 0.000000000000000000, -1.000000000000000000 ) ) ;
#2089 = CARTESIAN_POINT ( 'NONE',  ( -5.733772933379540859, 0.000000000000000000, -13.04554897075796660 ) ) ;
#2090 = DIRECTION ( 'NONE',  ( 0.000000000000000000, 0.000000000000000000, -1.000000000000000000 ) ) ;
#2091 = CARTESIAN_POINT ( 'NONE',  ( 2.453448243599949397, 0.1000000000000000056, -2.353846153846154365 ) ) ;
#2092 = AXIS2_PLACEMENT_3D ( 'NONE', #6235, #2858, #3957 ) ;
#2093 = CARTESIAN_POINT ( 'NONE',  ( -6.524296280129988190, 9.000000000000000000, -3.413039245436654490 ) ) ;
#2094 = CIRCLE ( 'NONE', #122, 1.500000000000000444 ) ;
#2095 = CARTESIAN_POINT ( 'NONE',  ( 12.08646469655232636, 3.000000000000000000, -8.883544964652022813 ) ) ;
#2096 = CARTESIAN_POINT ( 'NONE',  ( 5.051606143860418285, 1.734723475976807094E-15, 4.477027514692275112 ) ) ;
#2097 = VERTEX_POINT ( 'NONE', #6037 ) ;
#2098 = FACE_OUTER_BOUND ( 'NONE', #1133, .T. ) ;
#2099 = VERTEX_POINT ( 'NONE', #10241 ) ;
#2100 = EDGE_LOOP ( 'NONE', ( #2226, #8679 ) ) ;
#2101 = EDGE_CURVE ( 'NONE', #6340, #9161, #7137, .T. ) ;
#2102 = ORIENTED_EDGE ( 'NONE', *, *, #8983, .T. ) ;
#2103 = AXIS2_PLACEMENT_3D ( 'NONE', #9001, #13218, #13089 ) ;
#2104 = VERTEX_POINT ( 'NONE', #3325 ) ;
#2105 = CARTESIAN_POINT ( 'NONE',  ( 4.690415759823430619, 0.000000000000000000, 1.399999999999999911 ) ) ;
#2106 = CARTESIAN_POINT ( 'NONE',  ( 31.00000000000000000, 3.000000000000000000, 0.000000000000000000 ) ) ;
#2107 = DIRECTION ( 'NONE',  ( 0.8438162171727213723, 0.000000000000000000, -0.5366322685380732205 ) ) ;
#2108 = CARTESIAN_POINT ( 'NONE',  ( 12.37962962962963864, 3.000000000000000000, -12.43467921358330663 ) ) ;
#2109 = DIRECTION ( 'NONE',  ( -3.469446951953614189E-15, -1.000000000000000000, 0.000000000000000000 ) ) ;
#2110 = AXIS2_PLACEMENT_3D ( 'NONE', #756, #13289, #11080 ) ;
#2111 = CARTESIAN_POINT ( 'NONE',  ( -3.647470871583628593, 0.000000000000000000, 11.52666717836884125 ) ) ;
#2112 = ORIENTED_EDGE ( 'NONE', *, *, #198, .F. ) ;
#2113 = ORIENTED_EDGE ( 'NONE', *, *, #1970, .F. ) ;
#2114 = EDGE_CURVE ( 'NONE', #117, #4831, #9542, .T. ) ;
#2115 = ADVANCED_FACE ( 'NONE', ( #7539 ), #11890, .T. ) ;
#2116 = DIRECTION ( 'NONE',  ( 0.000000000000000000, 0.000000000000000000, -1.000000000000000000 ) ) ;
#2117 = ORIENTED_EDGE ( 'NONE', *, *, #10374, .T. ) ;
#2118 = DIRECTION ( 'NONE',  ( -0.000000000000000000, -1.000000000000000000, -0.000000000000000000 ) ) ;
#2119 = EDGE_CURVE ( 'NONE', #8226, #8945, #9223, .T. ) ;
#2120 = DIRECTION ( 'NONE',  ( -0.000000000000000000, -1.000000000000000000, -0.000000000000000000 ) ) ;
#2121 = PRODUCT_CONTEXT ( 'NONE', #8884, 'mechanical' ) ;
#2122 = DIRECTION ( 'NONE',  ( -0.000000000000000000, -1.000000000000000000, -0.000000000000000000 ) ) ;
#2123 = CARTESIAN_POINT ( 'NONE',  ( 9.573149624528804580, 3.000000000000000000, -8.795158114916638681 ) ) ;
#2124 = CARTESIAN_POINT ( 'NONE',  ( -12.68816982652953840, 3.000000000000000000, -2.830255545554093644 ) ) ;
#2125 = CARTESIAN_POINT ( 'NONE',  ( -10.97318381393799136, 3.000000000000000000, -6.970598036433411693 ) ) ;
#2126 = LINE ( 'NONE', #11835, #8430 ) ;
#2127 = ADVANCED_FACE ( 'NONE', ( #11745 ), #6083, .F. ) ;
#2128 = ORIENTED_EDGE ( 'NONE', *, *, #2703, .T. ) ;
#2129 = EDGE_LOOP ( 'NONE', ( #9631, #8673, #12095, #3001 ) ) ;
#2130 = VERTEX_POINT ( 'NONE', #10710 ) ;
#2131 = CARTESIAN_POINT ( 'NONE',  ( -0.5398653231797316820, 3.000000000000000000, 12.07794044664754018 ) ) ;
#2132 = ORIENTED_EDGE ( 'NONE', *, *, #8959, .T. ) ;
#2133 = EDGE_CURVE ( 'NONE', #13368, #2399, #8219, .T. ) ;
#2134 = DIRECTION ( 'NONE',  ( -0.000000000000000000, -1.000000000000000000, -0.000000000000000000 ) ) ;
#2135 = B_SPLINE_SURFACE_WITH_KNOTS ( 'NONE', 3, 1, ( 
 ( #4543, #6477 ),
 ( #10613, #10685 ),
 ( #1305, #9641 ),
 ( #4406, #6682 ) ),
 .UNSPECIFIED., .F., .F., .F.,
 ( 4, 4 ),
 ( 2, 2 ),
 ( 0.000000000000000000, 0.5855695330273008592 ),
 ( 0.000000000000000000, 1.000000000000000000 ),
 .UNSPECIFIED. ) ;
#2136 = CARTESIAN_POINT ( 'NONE',  ( 6.554160776451332104, 1.734723475976807094E-15, -1.614148852004323231 ) ) ;
#2137 = CARTESIAN_POINT ( 'NONE',  ( 13.50000000000000355, 0.000000000000000000, -5.550000000000001599 ) ) ;
#2138 = DIRECTION ( 'NONE',  ( -0.000000000000000000, -1.000000000000000000, -0.000000000000000000 ) ) ;
#2139 = CARTESIAN_POINT ( 'NONE',  ( 0.000000000000000000, 9.000000000000000000, 0.000000000000000000 ) ) ;
#2140 = LINE ( 'NONE', #5238, #4952 ) ;
#2141 = EDGE_LOOP ( 'NONE', ( #5853, #2424 ) ) ;
#2142 = CARTESIAN_POINT ( 'NONE',  ( 0.000000000000000000, 0.000000000000000000, 0.000000000000000000 ) ) ;
#2143 = ORIENTED_EDGE ( 'NONE', *, *, #7450, .T. ) ;
#2144 = ORIENTED_EDGE ( 'NONE', *, *, #7522, .T. ) ;
#2145 = EDGE_CURVE ( 'NONE', #6080, #1742, #5459, .T. ) ;
#2146 = ORIENTED_EDGE ( 'NONE', *, *, #9861, .F. ) ;
#2147 = CARTESIAN_POINT ( 'NONE',  ( 2.623034112301249721, 9.000000000000000000, -7.496701717520498853 ) ) ;
#2149 = VERTEX_POINT ( 'NONE', #4303 ) ;
#2148 = B_SPLINE_CURVE_WITH_KNOTS ( 'NONE', 3,
 ( #6724, #333, #6658, #3621 ),
 .UNSPECIFIED., .F., .F.,
 ( 4, 4 ),
 ( 0.1547128134717859205, 1.000000000000000000 ),
 .UNSPECIFIED. ) ;
#2150 = EDGE_CURVE ( 'NONE', #3649, #5599, #3256, .T. ) ;
#2151 = PLANE ( 'NONE',  #2311 ) ;
#2152 = CARTESIAN_POINT ( 'NONE',  ( 8.914835885878220623, 3.000000000000000000, -11.11702303352196708 ) ) ;
#2153 = CARTESIAN_POINT ( 'NONE',  ( 13.50000000000000355, 0.000000000000000000, -7.050000000000000711 ) ) ;
#2154 = LINE ( 'NONE', #5315, #7062 ) ;
#2155 = CARTESIAN_POINT ( 'NONE',  ( -2.546103534247749600, 0.000000000000000000, 12.55526518755974585 ) ) ;
#2156 = DIRECTION ( 'NONE',  ( 0.000000000000000000, 1.000000000000000000, 0.000000000000000000 ) ) ;
#2157 = B_SPLINE_SURFACE_WITH_KNOTS ( 'NONE', 3, 1, ( 
 ( #3066, #7343 ),
 ( #5141, #6438 ),
 ( #4309, #7474 ),
 ( #12654, #6300 ) ),
 .UNSPECIFIED., .F., .F., .F.,
 ( 4, 4 ),
 ( 2, 2 ),
 ( 0.1547128134717859205, 1.000000000000000000 ),
 ( 0.000000000000000000, 1.000000000000000000 ),
 .UNSPECIFIED. ) ;
#2158 = CARTESIAN_POINT ( 'NONE',  ( 13.54609072798131209, 3.000000000000000000, 3.536018380791111415 ) ) ;
#2159 = DIRECTION ( 'NONE',  ( 0.000000000000000000, 1.000000000000000000, -0.000000000000000000 ) ) ;
#2160 = ORIENTED_EDGE ( 'NONE', *, *, #61, .T. ) ;
#2161 = DIRECTION ( 'NONE',  ( 0.000000000000000000, 0.000000000000000000, -1.000000000000000000 ) ) ;
#2162 = ORIENTED_EDGE ( 'NONE', *, *, #12261, .F. ) ;
#2163 = EDGE_CURVE ( 'NONE', #10097, #12683, #11083, .T. ) ;
#2164 = PRODUCT_DEFINITION_SHAPE ( 'NONE', 'NONE',  #13600 ) ;
#2165 = ORIENTED_EDGE ( 'NONE', *, *, #11291, .T. ) ;
#2166 = ORIENTED_EDGE ( 'NONE', *, *, #8840, .F. ) ;
#2167 = CARTESIAN_POINT ( 'NONE',  ( -14.90895795148409420, 0.000000000000000000, 1.650143266773909101 ) ) ;
#2168 = DIRECTION ( 'NONE',  ( 0.000000000000000000, 0.000000000000000000, 1.000000000000000000 ) ) ;
#2169 = DIRECTION ( 'NONE',  ( 0.6291930273683260522, 0.000000000000000000, -0.7772490812545749250 ) ) ;
#2170 = CARTESIAN_POINT ( 'NONE',  ( 0.000000000000000000, 3.000000000000000000, 0.000000000000000000 ) ) ;
#2171 = PLANE ( 'NONE',  #12135 ) ;
#2172 = EDGE_CURVE ( 'NONE', #7190, #10761, #1208, .T. ) ;
#2173 = B_SPLINE_CURVE_WITH_KNOTS ( 'NONE', 3,
 ( #11816, #8826, #13050, #2579 ),
 .UNSPECIFIED., .F., .F.,
 ( 4, 4 ),
 ( 0.000000000000000000, 0.5855695330273008592 ),
 .UNSPECIFIED. ) ;
#2174 = DIRECTION ( 'NONE',  ( 0.000000000000000000, 1.000000000000000000, -0.000000000000000000 ) ) ;
#2175 = ORIENTED_EDGE ( 'NONE', *, *, #3801, .F. ) ;
#2176 = ORIENTED_EDGE ( 'NONE', *, *, #10005, .T. ) ;
#2177 = CARTESIAN_POINT ( 'NONE',  ( 0.000000000000000000, 0.09999999999999982514, 1.600000000000000311 ) ) ;
#2178 = ORIENTED_EDGE ( 'NONE', *, *, #6674, .T. ) ;
#2179 = CARTESIAN_POINT ( 'NONE',  ( -14.82803603298502360, 0.000000000000000000, -2.264806262022826644 ) ) ;
#2180 = DIRECTION ( 'NONE',  ( -0.000000000000000000, -1.000000000000000000, -0.000000000000000000 ) ) ;
#2181 = CARTESIAN_POINT ( 'NONE',  ( 7.494008246337245716, 0.000000000000000000, -11.63517940784380578 ) ) ;
#2182 = CARTESIAN_POINT ( 'NONE',  ( 2.604531154829233586, 0.000000000000000000, 11.80612203322752585 ) ) ;
#2183 = AXIS2_PLACEMENT_3D ( 'NONE', #6797, #9897, #6873 ) ;
#2184 = EDGE_CURVE ( 'NONE', #11220, #1535, #10650, .T. ) ;
#2185 = DIRECTION ( 'NONE',  ( -1.000000000000000000, 3.469446951953610639E-15, 2.602085213965210149E-16 ) ) ;
#2186 = DIRECTION ( 'NONE',  ( 0.000000000000000000, 0.000000000000000000, 1.000000000000000000 ) ) ;
#2187 = LINE ( 'NONE', #11973, #6238 ) ;
#2188 = ORIENTED_EDGE ( 'NONE', *, *, #4381, .F. ) ;
#2189 = ORIENTED_EDGE ( 'NONE', *, *, #12522, .F. ) ;
#2190 = ORIENTED_EDGE ( 'NONE', *, *, #6830, .T. ) ;
#2191 = LINE ( 'NONE', #13571, #2255 ) ;
#2192 = ORIENTED_EDGE ( 'NONE', *, *, #5665, .F. ) ;
#2193 = CARTESIAN_POINT ( 'NONE',  ( -8.352599575481690408, 3.000000000000000000, 30.99999999999999289 ) ) ;
#2194 = EDGE_CURVE ( 'NONE', #9874, #11321, #682, .T. ) ;
#2195 = CYLINDRICAL_SURFACE ( 'NONE', #9895, 9.250000000000000000 ) ;
#2196 = EDGE_CURVE ( 'NONE', #12802, #20, #1825, .T. ) ;
#2197 = LINE ( 'NONE', #87, #101 ) ;
#2198 = CARTESIAN_POINT ( 'NONE',  ( 0.000000000000000000, 3.000000000000000000, 0.000000000000000000 ) ) ;
#2199 = AXIS2_PLACEMENT_3D ( 'NONE', #2091, #5252, #4149 ) ;
#2200 = LINE ( 'NONE', #350, #9712 ) ;
#2201 = AXIS2_PLACEMENT_3D ( 'NONE', #1240, #5431, #12 ) ;
#2202 = DIRECTION ( 'NONE',  ( 0.000000000000000000, 0.000000000000000000, 1.000000000000000000 ) ) ;
#2203 = ORIENTED_EDGE ( 'NONE', *, *, #4595, .T. ) ;
#2204 = ADVANCED_FACE ( 'NONE', ( #11813, #47, #9465 ), #11610, .F. ) ;
#2205 =( NAMED_UNIT ( * ) SI_UNIT ( $, .STERADIAN. ) SOLID_ANGLE_UNIT ( ) );
#2206 = ORIENTED_EDGE ( 'NONE', *, *, #6575, .F. ) ;
#2207 = EDGE_CURVE ( 'NONE', #10329, #13219, #6735, .T. ) ;
#2208 = VERTEX_POINT ( 'NONE', #7409 ) ;
#2209 = ORIENTED_EDGE ( 'NONE', *, *, #5475, .F. ) ;
#2210 = CARTESIAN_POINT ( 'NONE',  ( -6.025412986832177076, 3.000000000000000000, -13.73660796332610268 ) ) ;
#2211 = B_SPLINE_CURVE_WITH_KNOTS ( 'NONE', 3,
 ( #169, #5586, #11930, #4557 ),
 .UNSPECIFIED., .F., .F.,
 ( 4, 4 ),
 ( 0.1547128134717859205, 1.000000000000000000 ),
 .UNSPECIFIED. ) ;
#2212 = VERTEX_POINT ( 'NONE', #435 ) ;
#2213 = AXIS2_PLACEMENT_3D ( 'NONE', #2878, #758, #8114 ) ;
#2214 = AXIS2_PLACEMENT_3D ( 'NONE', #12601, #70, #1284 ) ;
#2215 = FACE_OUTER_BOUND ( 'NONE', #10799, .T. ) ;
#2216 = CARTESIAN_POINT ( 'NONE',  ( 53.78299299645824050, 3.000000000000000000, -4.528231303176834643 ) ) ;
#2217 = EDGE_CURVE ( 'NONE', #11316, #11354, #9554, .T. ) ;
#2218 = DIRECTION ( 'NONE',  ( 0.000000000000000000, 0.000000000000000000, 1.000000000000000000 ) ) ;
#2219 = DIRECTION ( 'NONE',  ( -0.000000000000000000, -1.000000000000000000, -0.000000000000000000 ) ) ;
#2220 = CARTESIAN_POINT ( 'NONE',  ( 2.264806262022877714, 0.000000000000000000, -14.82803603298501471 ) ) ;
#2221 = DIRECTION ( 'NONE',  ( -0.000000000000000000, -1.000000000000000000, -0.000000000000000000 ) ) ;
#2222 = CARTESIAN_POINT ( 'NONE',  ( -9.573149624528719315, 3.000000000000000000, -8.795158114916407754 ) ) ;
#2223 = ORIENTED_EDGE ( 'NONE', *, *, #346, .F. ) ;
#2224 = CARTESIAN_POINT ( 'NONE',  ( 5.958322434183389582, 9.000000000000000000, -6.062045345451230638 ) ) ;
#2225 = AXIS2_PLACEMENT_3D ( 'NONE', #10092, #2795, #11271 ) ;
#2226 = ORIENTED_EDGE ( 'NONE', *, *, #10278, .F. ) ;
#2227 = ORIENTED_EDGE ( 'NONE', *, *, #3550, .F. ) ;
#2228 = EDGE_LOOP ( 'NONE', ( #10791, #2911, #11622, #2887 ) ) ;
#2229 = CARTESIAN_POINT ( 'NONE',  ( -6.934601996837493232, 9.000000000000000000, 3.871968458191308748 ) ) ;
#2230 = DIRECTION ( 'NONE',  ( 0.000000000000000000, 0.000000000000000000, -1.000000000000000000 ) ) ;
#2231 = EDGE_CURVE ( 'NONE', #9010, #7333, #4707, .T. ) ;
#2232 = EDGE_CURVE ( 'NONE', #7353, #5239, #8757, .T. ) ;
#2233 = PLANE ( 'NONE',  #13273 ) ;
#2234 = LINE ( 'NONE', #10653, #9228 ) ;
#2235 = CARTESIAN_POINT ( 'NONE',  ( -11.90284147956865723, 0.000000000000000000, -9.133371500908332052 ) ) ;
#2236 = B_SPLINE_CURVE_WITH_KNOTS ( 'NONE', 3,
 ( #12874, #3419, #5556, #3153 ),
 .UNSPECIFIED., .F., .F.,
 ( 4, 4 ),
 ( 0.000000000000000000, 0.5855695330273008592 ),
 .UNSPECIFIED. ) ;
#2237 = CARTESIAN_POINT ( 'NONE',  ( 30.79786191028635400, 3.000000000000000000, -6.999232361977355765 ) ) ;
#2238 = ORIENTED_EDGE ( 'NONE', *, *, #4761, .F. ) ;
#2239 = VERTEX_POINT ( 'NONE', #10842 ) ;
#2240 = CARTESIAN_POINT ( 'NONE',  ( 31.00000000000000000, 0.000000000000000000, 0.000000000000000000 ) ) ;
#2241 = B_SPLINE_SURFACE_WITH_KNOTS ( 'NONE', 3, 1, ( 
 ( #13553, #1979 ),
 ( #10311, #7009 ),
 ( #4941, #1847 ),
 ( #10168, #13279 ) ),
 .UNSPECIFIED., .F., .F., .F.,
 ( 4, 4 ),
 ( 2, 2 ),
 ( 0.000000000000000000, 0.8452273900860258760 ),
 ( 0.000000000000000000, 1.000000000000000000 ),
 .UNSPECIFIED. ) ;
#2242 = ORIENTED_EDGE ( 'NONE', *, *, #11661, .T. ) ;
#2243 = CARTESIAN_POINT ( 'NONE',  ( 0.000000000000000000, 9.000000000000000000, 0.000000000000000000 ) ) ;
#2244 = DIRECTION ( 'NONE',  ( 0.000000000000000000, 0.000000000000000000, 1.000000000000000000 ) ) ;
#2245 = VECTOR ( 'NONE', #9815, 1000.000000000000000 ) ;
#2246 = CIRCLE ( 'NONE', #285, 1.000000000000000000 ) ;
#2247 = AXIS2_PLACEMENT_3D ( 'NONE', #12014, #2569, #13172 ) ;
#2248 = CARTESIAN_POINT ( 'NONE',  ( 47.14458624375820506, 3.000000000000000000, -3.829406728833672613 ) ) ;
#2249 = DIRECTION ( 'NONE',  ( 0.000000000000000000, 1.000000000000000000, 0.000000000000000000 ) ) ;
#2250 = DIRECTION ( 'NONE',  ( -3.469446951953610639E-15, -1.000000000000000000, 0.000000000000000000 ) ) ;
#2251 = CARTESIAN_POINT ( 'NONE',  ( 2.264806262022877714, 0.000000000000000000, -14.82803603298501471 ) ) ;
#2252 = CARTESIAN_POINT ( 'NONE',  ( 3.818534268238711782, 0.000000000000000000, -5.566084444408534004 ) ) ;
#2253 = VERTEX_POINT ( 'NONE', #506 ) ;
#2254 = VERTEX_POINT ( 'NONE', #7933 ) ;
#2255 = VECTOR ( 'NONE', #6389, 1000.000000000000000 ) ;
#2256 = ORIENTED_EDGE ( 'NONE', *, *, #4060, .F. ) ;
#2257 = CARTESIAN_POINT ( 'NONE',  ( 1.557181465540758758, 0.000000000000000000, 14.16466328168009881 ) ) ;
#2258 = VECTOR ( 'NONE', #7072, 1000.000000000000000 ) ;
#2259 = AXIS2_PLACEMENT_3D ( 'NONE', #4077, #5105, #11443 ) ;
#2260 = ADVANCED_FACE ( 'NONE', ( #7732 ), #13249, .T. ) ;
#2261 = VERTEX_POINT ( 'NONE', #11947 ) ;
#2262 = CARTESIAN_POINT ( 'NONE',  ( 9.573149624528804580, 3.000000000000000000, -8.795158114916638681 ) ) ;
#2263 = DIRECTION ( 'NONE',  ( 0.000000000000000000, 1.000000000000000000, -0.000000000000000000 ) ) ;
#2264 = VECTOR ( 'NONE', #6097, 1000.000000000000000 ) ;
#2265 = LINE ( 'NONE', #349, #1852 ) ;
#2266 = PRODUCT_DEFINITION_SHAPE ( 'NONE', 'NONE',  #13611 ) ;
#2267 = CARTESIAN_POINT ( 'NONE',  ( 13.54609072798131209, 0.000000000000000000, 3.536018380791111415 ) ) ;
#2268 = VECTOR ( 'NONE', #13335, 1000.000000000000000 ) ;
#2269 = AXIS2_PLACEMENT_3D ( 'NONE', #12185, #1497, #12999 ) ;
#2270 = DIRECTION ( 'NONE',  ( -0.000000000000000000, -1.000000000000000000, -0.000000000000000000 ) ) ;
#2271 = DIRECTION ( 'NONE',  ( -0.000000000000000000, -1.000000000000000000, -0.000000000000000000 ) ) ;
#2272 = AXIS2_PLACEMENT_3D ( 'NONE', #8521, #6469, #9573 ) ;
#2273 = ORIENTED_EDGE ( 'NONE', *, *, #10801, .F. ) ;
#2274 = ORIENTED_EDGE ( 'NONE', *, *, #1537, .F. ) ;
#2275 = ORIENTED_EDGE ( 'NONE', *, *, #8478, .T. ) ;
#2276 = ORIENTED_EDGE ( 'NONE', *, *, #4306, .T. ) ;
#2277 = CARTESIAN_POINT ( 'NONE',  ( 48.80418793193314997, 0.000000000000000000, -4.004112872419501201 ) ) ;
#2278 = EDGE_CURVE ( 'NONE', #2254, #7268, #10593, .T. ) ;
#2279 = EDGE_CURVE ( 'NONE', #11521, #10836, #6906, .T. ) ;
#2280 = ORIENTED_EDGE ( 'NONE', *, *, #10025, .F. ) ;
#2281 = VECTOR ( 'NONE', #9666, 1000.000000000000000 ) ;
#2283 = EDGE_CURVE ( 'NONE', #10892, #10734, #2720, .T. ) ;
#2282 = CIRCLE ( 'NONE', #10203, 1.500000000000001332 ) ;
#2284 = DIRECTION ( 'NONE',  ( 0.9893737785712105604, -0.000000000000000000, -0.1453943818575020863 ) ) ;
#2285 = EDGE_CURVE ( 'NONE', #3746, #10516, #3395, .T. ) ;
#2286 = CARTESIAN_POINT ( 'NONE',  ( 8.795158114916441505, 0.000000000000000000, -9.573149624528689117 ) ) ;
#2287 = ADVANCED_FACE ( 'NONE', ( #11115 ), #5732, .F. ) ;
#2288 = DIRECTION ( 'NONE',  ( -0.000000000000000000, -1.000000000000000000, -0.000000000000000000 ) ) ;
#2289 = CARTESIAN_POINT ( 'NONE',  ( -8.158551673544545579, 0.000000000000000000, 8.922226997226644585 ) ) ;
#2290 = CARTESIAN_POINT ( 'NONE',  ( 6.343080161942737938, 3.000000000000000000, -11.35348358516942469 ) ) ;
#2291 = LINE ( 'NONE', #6494, #9092 ) ;
#2292 = DIRECTION ( 'NONE',  ( -0.000000000000000000, -1.000000000000000000, -0.000000000000000000 ) ) ;
#2293 = CARTESIAN_POINT ( 'NONE',  ( 0.000000000000000000, 3.000000000000000000, 5.000000000000000000 ) ) ;
#2294 = ORIENTED_EDGE ( 'NONE', *, *, #8948, .F. ) ;
#2295 = AXIS2_PLACEMENT_3D ( 'NONE', #11971, #1709, #668 ) ;
#2296 = CARTESIAN_POINT ( 'NONE',  ( 6.660877044263387781, 0.000000000000000000, -11.16999893002129696 ) ) ;
#2297 = CIRCLE ( 'NONE', #8450, 0.09999999999999982514 ) ;
#2298 = B_SPLINE_CURVE_WITH_KNOTS ( 'NONE', 3,
 ( #10242, #13270, #3829, #10304 ),
 .UNSPECIFIED., .F., .F.,
 ( 4, 4 ),
 ( 0.000000000000000000, 0.5855695330273008592 ),
 .UNSPECIFIED. ) ;
#2299 = ORIENTED_EDGE ( 'NONE', *, *, #795, .T. ) ;
#2300 = EDGE_LOOP ( 'NONE', ( #3209, #7876, #1458, #4515 ) ) ;
#2301 =( REPRESENTATION_RELATIONSHIP ('NONE','NONE', #3798, #8461 ) REPRESENTATION_RELATIONSHIP_WITH_TRANSFORMATION ( #12234 )SHAPE_REPRESENTATION_RELATIONSHIP( ) );
#2302 = EDGE_CURVE ( 'NONE', #11220, #9600, #5274, .T. ) ;
#2303 = ORIENTED_EDGE ( 'NONE', *, *, #9275, .F. ) ;
#2304 = EDGE_CURVE ( 'NONE', #11250, #6484, #11758, .T. ) ;
#2305 = B_SPLINE_CURVE_WITH_KNOTS ( 'NONE', 3,
 ( #6119, #2807, #7016, #9208 ),
 .UNSPECIFIED., .F., .F.,
 ( 4, 4 ),
 ( 0.000000000000000000, 0.5855695330273008592 ),
 .UNSPECIFIED. ) ;
#2306 = CARTESIAN_POINT ( 'NONE',  ( -13.82336506795071607, 0.000000000000000000, 0.6724118135763649251 ) ) ;
#2307 = VECTOR ( 'NONE', #11268, 1000.000000000000000 ) ;
#2308 = AXIS2_PLACEMENT_3D ( 'NONE', #10702, #2567, #6698 ) ;
#2309 = CARTESIAN_POINT ( 'NONE',  ( -8.890701948131944476, 0.000000000000000000, 13.39999999999999858 ) ) ;
#2310 = EDGE_CURVE ( 'NONE', #5342, #5243, #4489, .T. ) ;
#2311 = AXIS2_PLACEMENT_3D ( 'NONE', #5383, #11724, #2356 ) ;
#2312 = PLANE ( 'NONE',  #8209 ) ;
#2313 = CARTESIAN_POINT ( 'NONE',  ( -1.650143266773857142, 3.000000000000000000, -14.90895795148409952 ) ) ;
#2314 = CARTESIAN_POINT ( 'NONE',  ( -8.222660081691577361, 0.000000000000000000, -8.549999999999998934 ) ) ;
#2315 = CARTESIAN_POINT ( 'NONE',  ( 0.000000000000000000, 3.000000000000000000, 0.000000000000000000 ) ) ;
#2316 = ORIENTED_EDGE ( 'NONE', *, *, #6450, .F. ) ;
#2317 = VECTOR ( 'NONE', #168, 1000.000000000000000 ) ;
#2318 = CIRCLE ( 'NONE', #1894, 1.000000000000000888 ) ;
#2319 = EDGE_LOOP ( 'NONE', ( #8530, #11983, #7800, #3488 ) ) ;
#2320 = EDGE_CURVE ( 'NONE', #11192, #5918, #1495, .T. ) ;
#2321 = CARTESIAN_POINT ( 'NONE',  ( 3.850308450823737960, 9.000000000000000000, 5.544152309732778505 ) ) ;
#2322 = EDGE_CURVE ( 'NONE', #8945, #6374, #9032, .T. ) ;
#2323 = SHAPE_REPRESENTATION ( 'gear-link-1', ( #10007 ), #5843 ) ;
#2324 = EDGE_LOOP ( 'NONE', ( #8109, #5994, #3687, #3675 ) ) ;
#2325 = B_SPLINE_CURVE_WITH_KNOTS ( 'NONE', 3,
 ( #9684, #11969, #12932, #10927 ),
 .UNSPECIFIED., .F., .F.,
 ( 4, 4 ),
 ( 0.000000000000000000, 0.5855695330273008592 ),
 .UNSPECIFIED. ) ;
#2326 = DIRECTION ( 'NONE',  ( 0.000000000000000000, 0.000000000000000000, -1.000000000000000000 ) ) ;
#2327 = DIRECTION ( 'NONE',  ( 3.469446951953610639E-15, 1.000000000000000000, 2.891205793294675861E-16 ) ) ;
#2328 = DIRECTION ( 'NONE',  ( 0.000000000000000000, 0.000000000000000000, 1.000000000000000000 ) ) ;
#2329 = CARTESIAN_POINT ( 'NONE',  ( -6.343077614891082128, 3.000000000000000000, -11.35348748332310720 ) ) ;
#2330 = CARTESIAN_POINT ( 'NONE',  ( -13.86115248177182835, 0.000000000000000000, -5.741477348071267528 ) ) ;
#2331 = CARTESIAN_POINT ( 'NONE',  ( 0.000000000000000000, 0.000000000000000000, 0.000000000000000000 ) ) ;
#2332 = CARTESIAN_POINT ( 'NONE',  ( 4.072642252455978884, 3.000000000000000000, 12.14623037080101042 ) ) ;
#2333 = ORIENTED_EDGE ( 'NONE', *, *, #10801, .T. ) ;
#2334 = EDGE_CURVE ( 'NONE', #9307, #12420, #4570, .T. ) ;
#2335 = VERTEX_POINT ( 'NONE', #1475 ) ;
#2336 = PRODUCT_CONTEXT ( 'NONE', #3509, 'mechanical' ) ;
#2337 = ORIENTED_EDGE ( 'NONE', *, *, #9364, .F. ) ;
#2338 = CARTESIAN_POINT ( 'NONE',  ( 8.914835885878215294, 3.000000000000000000, 11.11702303352197418 ) ) ;
#2339 = ORIENTED_EDGE ( 'NONE', *, *, #7209, .F. ) ;
#2340 = DIRECTION ( 'NONE',  ( 0.000000000000000000, 1.000000000000000000, 0.000000000000000000 ) ) ;
#2341 = CARTESIAN_POINT ( 'NONE',  ( 30.82048254704846713, 3.000000000000000000, -7.998976482636475538 ) ) ;
#2342 = CARTESIAN_POINT ( 'NONE',  ( -11.48836750521723893, 3.000000000000000000, 8.430890348300625448 ) ) ;
#2343 = DIRECTION ( 'NONE',  ( 0.000000000000000000, 0.000000000000000000, -1.000000000000000000 ) ) ;
#2344 = CARTESIAN_POINT ( 'NONE',  ( 10.00000000000002309, 8.000000000000007105, 7.000000000000001776 ) ) ;
#2345 = CYLINDRICAL_SURFACE ( 'NONE', #562, 12.08999999999737440 ) ;
#2346 = EDGE_CURVE ( 'NONE', #3691, #8949, #4938, .T. ) ;
#2347 = VERTEX_POINT ( 'NONE', #7802 ) ;
#2348 = CARTESIAN_POINT ( 'NONE',  ( 7.940744365623959133, 9.000000000000000000, 0.1715058177969961128 ) ) ;
#2349 = VERTEX_POINT ( 'NONE', #12371 ) ;
#2350 = ORIENTED_EDGE ( 'NONE', *, *, #6212, .T. ) ;
#2351 = EDGE_LOOP ( 'NONE', ( #6981, #2596, #6036, #2146 ) ) ;
#2352 = CARTESIAN_POINT ( 'NONE',  ( -13.00394572736061605, 0.000000000000000000, 0.1835083749157108701 ) ) ;
#2353 = VERTEX_POINT ( 'NONE', #13459 ) ;
#2354 = VERTEX_POINT ( 'NONE', #6983 ) ;
#2355 = B_SPLINE_CURVE_WITH_KNOTS ( 'NONE', 3,
 ( #7300, #1032, #2069, #9426 ),
 .UNSPECIFIED., .F., .F.,
 ( 4, 4 ),
 ( 0.6363612417694253232, 0.6657793188270956231 ),
 .UNSPECIFIED. ) ;
#2356 = DIRECTION ( 'NONE',  ( -1.000000000000000000, 0.000000000000000000, -0.000000000000000000 ) ) ;
#2357 =( LENGTH_UNIT ( ) NAMED_UNIT ( * ) SI_UNIT ( .MILLI., .METRE. ) );
#2358 = LINE ( 'NONE', #5447, #6645 ) ;
#2359 = CARTESIAN_POINT ( 'NONE',  ( -8.883544964652065445, 3.000000000000000000, -12.08646469655229438 ) ) ;
#2360 = CARTESIAN_POINT ( 'NONE',  ( 2.414978278956333213, 0.000000000000000000, -13.33788847341978645 ) ) ;
#2361 = CARTESIAN_POINT ( 'NONE',  ( 4.690415759823430619, 3.000000000000000000, 4.500000000000000888 ) ) ;
#2362 = DIRECTION ( 'NONE',  ( 0.000000000000000000, 0.000000000000000000, 1.000000000000000000 ) ) ;
#2363 = EDGE_CURVE ( 'NONE', #375, #2349, #3043, .T. ) ;
#2364 = EDGE_LOOP ( 'NONE', ( #8853, #13343, #7550, #4962 ) ) ;
#2365 = ADVANCED_FACE ( 'NONE', ( #7127, #10285, #8279 ), #4084, .T. ) ;
#2366 = CARTESIAN_POINT ( 'NONE',  ( 6.343080161942737938, 0.000000000000000000, -11.35348358516942469 ) ) ;
#2367 = B_SPLINE_SURFACE_WITH_KNOTS ( 'NONE', 3, 1, ( 
 ( #13220, #4683 ),
 ( #4609, #12203 ),
 ( #12060, #11157 ),
 ( #2754, #1727 ) ),
 .UNSPECIFIED., .F., .F., .F.,
 ( 4, 4 ),
 ( 2, 2 ),
 ( 0.000000000000000000, 0.8452273900860258760 ),
 ( 0.000000000000000000, 1.000000000000000000 ),
 .UNSPECIFIED. ) ;
#2368 = ORIENTED_EDGE ( 'NONE', *, *, #5983, .F. ) ;
#2369 = CIRCLE ( 'NONE', #5444, 12.08999999999737440 ) ;
#2370 = VERTEX_POINT ( 'NONE', #6087 ) ;
#2371 = ORIENTED_EDGE ( 'NONE', *, *, #10453, .F. ) ;
#2372 = CARTESIAN_POINT ( 'NONE',  ( 7.758214145541979967, 9.000000000000000000, 1.700281702449083054 ) ) ;
#2373 = CARTESIAN_POINT ( 'NONE',  ( 8.481367827640703183, 0.000000000000000000, 0.5624942419805130100 ) ) ;
#2374 = EDGE_CURVE ( 'NONE', #2415, #3742, #4270, .T. ) ;
#2375 = CARTESIAN_POINT ( 'NONE',  ( -0.5400000000007666445, 3.000000000000000000, -12.07793442604883793 ) ) ;
#2376 = CARTESIAN_POINT ( 'NONE',  ( -11.70905276178463872, 3.000000000000000000, -9.375397774054366806 ) ) ;
#2377 = CARTESIAN_POINT ( 'NONE',  ( 0.000000000000000000, 3.000000000000000000, 0.000000000000000000 ) ) ;
#2378 = VERTEX_POINT ( 'NONE', #850 ) ;
#2379 = EDGE_CURVE ( 'NONE', #594, #3134, #3609, .T. ) ;
#2380 = VERTEX_POINT ( 'NONE', #4010 ) ;
#2381 = EDGE_CURVE ( 'NONE', #3023, #4625, #13086, .T. ) ;
#2382 = CARTESIAN_POINT ( 'NONE',  ( 8.252687871541644071, 3.000000000000000000, 28.00000000000000000 ) ) ;
#2384 = ORIENTED_EDGE ( 'NONE', *, *, #12315, .F. ) ;
#2383 = B_SPLINE_CURVE_WITH_KNOTS ( 'NONE', 3,
 ( #2089, #12566, #11452, #6218 ),
 .UNSPECIFIED., .F., .F.,
 ( 4, 4 ),
 ( 0.000000000000000000, 0.8452273900860258760 ),
 .UNSPECIFIED. ) ;
#2385 = CARTESIAN_POINT ( 'NONE',  ( 52.12339130828321032, 0.000000000000000000, -4.353525159591052685 ) ) ;
#2386 = CYLINDRICAL_SURFACE ( 'NONE', #12106, 4.390701948131951582 ) ;
#2387 = DIRECTION ( 'NONE',  ( 0.000000000000000000, 0.000000000000000000, -1.000000000000000000 ) ) ;
#2388 = EDGE_CURVE ( 'NONE', #11595, #10663, #6143, .T. ) ;
#2389 = DIRECTION ( 'NONE',  ( -0.000000000000000000, -1.000000000000000000, -0.000000000000000000 ) ) ;
#2390 = DIRECTION ( 'NONE',  ( 0.000000000000000000, 1.000000000000000000, 0.000000000000000000 ) ) ;
#2391 = CARTESIAN_POINT ( 'NONE',  ( 31.00000000000000000, 0.09999999999999982514, 3.399999999999999911 ) ) ;
#2392 = CARTESIAN_POINT ( 'NONE',  ( 41.67875868938293138, 0.000000000000000000, -6.066649533482935119 ) ) ;
#2393 = CYLINDRICAL_SURFACE ( 'NONE', #4693, 6.750000000000000888 ) ;
#2394 = ORIENTED_EDGE ( 'NONE', *, *, #444, .F. ) ;
#2395 = ORIENTED_EDGE ( 'NONE', *, *, #8983, .F. ) ;
#2396 = ORIENTED_EDGE ( 'NONE', *, *, #7136, .T. ) ;
#2397 = VERTEX_POINT ( 'NONE', #12564 ) ;
#2398 = CARTESIAN_POINT ( 'NONE',  ( 12.08646469655232636, 0.000000000000000000, -8.883544964652022813 ) ) ;
#2399 = VERTEX_POINT ( 'NONE', #10346 ) ;
#2400 = DIRECTION ( 'NONE',  ( -0.000000000000000000, -1.000000000000000000, -0.000000000000000000 ) ) ;
#2401 =( NAMED_UNIT ( * ) SI_UNIT ( $, .STERADIAN. ) SOLID_ANGLE_UNIT ( ) );
#2402 = EDGE_CURVE ( 'NONE', #1248, #11926, #8062, .T. ) ;
#2403 = CARTESIAN_POINT ( 'NONE',  ( 7.659717769608228366, 0.000000000000000000, -2.099897208369672530 ) ) ;
#2404 = PLANE ( 'NONE',  #983 ) ;
#2405 = LINE ( 'NONE', #7381, #12593 ) ;
#2406 = DIRECTION ( 'NONE',  ( -0.000000000000000000, -1.000000000000000000, -0.000000000000000000 ) ) ;
#2407 = B_SPLINE_CURVE_WITH_KNOTS ( 'NONE', 3,
 ( #2626, #6826, #10133, #6901 ),
 .UNSPECIFIED., .F., .F.,
 ( 4, 4 ),
 ( 0.1276832474596250877, 1.000000000000000000 ),
 .UNSPECIFIED. ) ;
#2408 = ORIENTED_EDGE ( 'NONE', *, *, #9087, .F. ) ;
#2409 = SURFACE_SIDE_STYLE ('',( #9581 ) ) ;
#2410 = ORIENTED_EDGE ( 'NONE', *, *, #4844, .F. ) ;
#2411 = ORIENTED_EDGE ( 'NONE', *, *, #8154, .T. ) ;
#2412 = ORIENTED_EDGE ( 'NONE', *, *, #5232, .F. ) ;
#2413 = DIRECTION ( 'NONE',  ( 0.9893737785712105604, 0.000000000000000000, -0.1453943818575021141 ) ) ;
#2414 = ORIENTED_EDGE ( 'NONE', *, *, #7339, .T. ) ;
#2415 = VERTEX_POINT ( 'NONE', #1892 ) ;
#2416 = CARTESIAN_POINT ( 'NONE',  ( -13.73660796332618261, 0.000000000000000000, -6.025412986832017204 ) ) ;
#2417 = CIRCLE ( 'NONE', #10989, 5.499999999999996447 ) ;
#2418 = DIRECTION ( 'NONE',  ( -0.000000000000000000, -1.000000000000000000, -0.000000000000000000 ) ) ;
#2419 = DIRECTION ( 'NONE',  ( 0.000000000000000000, 0.000000000000000000, 1.000000000000000000 ) ) ;
#2420 = AXIS2_PLACEMENT_3D ( 'NONE', #2918, #9592, #5385 ) ;
#2421 = CARTESIAN_POINT ( 'NONE',  ( 8.430890348300586368, 3.000000000000000000, -11.48836750521726913 ) ) ;
#2422 = CARTESIAN_POINT ( 'NONE',  ( -13.04554897075795949, 0.000000000000000000, 5.733772933379550629 ) ) ;
#2423 = DIRECTION ( 'NONE',  ( 0.5366322685380732205, 0.000000000000000000, 0.8438162171727212613 ) ) ;
#2424 = ORIENTED_EDGE ( 'NONE', *, *, #1124, .T. ) ;
#2425 = CARTESIAN_POINT ( 'NONE',  ( 10.14701493152832512, 0.000000000000000000, -29.73855628788322747 ) ) ;
#2426 = VERTEX_POINT ( 'NONE', #12443 ) ;
#2427 = ORIENTED_EDGE ( 'NONE', *, *, #1095, .T. ) ;
#2428 = CIRCLE ( 'NONE', #2860, 1.500000000000001332 ) ;
#2429 = AXIS2_PLACEMENT_3D ( 'NONE', #1528, #5587, #2618 ) ;
#2430 = ORIENTED_EDGE ( 'NONE', *, *, #6041, .T. ) ;
#2431 = EDGE_CURVE ( 'NONE', #4566, #7781, #13590, .T. ) ;
#2432 = CARTESIAN_POINT ( 'NONE',  ( 6.553553527263006551, 0.000000000000000000, 1.616612558808879774 ) ) ;
#2433 = CARTESIAN_POINT ( 'NONE',  ( -5.708888906988910605, 0.000000000000000000, 11.46847481510586597 ) ) ;
#2434 = ADVANCED_BREP_SHAPE_REPRESENTATION ( '', ( #4005, #10007 ), #6949 ) ;
#2435 = CONTEXT_DEPENDENT_SHAPE_REPRESENTATION ( #3431, #11964 ) ;
#2436 = DIRECTION ( 'NONE',  ( 0.000000000000000000, 1.000000000000000000, -0.000000000000000000 ) ) ;
#2437 = VECTOR ( 'NONE', #10525, 1000.000000000000000 ) ;
#2438 = DIRECTION ( 'NONE',  ( 0.000000000000000000, 1.000000000000000000, 0.000000000000000000 ) ) ;
#2439 = DIRECTION ( 'NONE',  ( -0.000000000000000000, -1.000000000000000000, -0.000000000000000000 ) ) ;
#2440 = VECTOR ( 'NONE', #9770, 1000.000000000000000 ) ;
#2441 = LINE ( 'NONE', #7810, #10166 ) ;
#2442 = EDGE_LOOP ( 'NONE', ( #1232, #11128, #3557, #3779 ) ) ;
#2443 = ORIENTED_EDGE ( 'NONE', *, *, #12580, .F. ) ;
#2444 = CARTESIAN_POINT ( 'NONE',  ( 4.821006024660968947, 3.000000000000000000, -13.61374091949021015 ) ) ;
#2445 = AXIS2_PLACEMENT_3D ( 'NONE', #9870, #7615, #6573 ) ;
#2446 = EDGE_CURVE ( 'NONE', #3500, #6704, #553, .T. ) ;
#2447 = EDGE_CURVE ( 'NONE', #9461, #8060, #5112, .T. ) ;
#2448 = VERTEX_POINT ( 'NONE', #1749 ) ;
#2449 = CARTESIAN_POINT ( 'NONE',  ( -11.11702303352192445, 0.000000000000000000, 8.914835885878272137 ) ) ;
#2450 = DIRECTION ( 'NONE',  ( 1.000000000000000000, 0.000000000000000000, -0.000000000000000000 ) ) ;
#2451 = ADVANCED_FACE ( 'NONE', ( #8079 ), #4145, .T. ) ;
#2452 = CARTESIAN_POINT ( 'NONE',  ( -11.11702303352197063, 3.000000000000000000, -8.914835885878215294 ) ) ;
#2453 = ADVANCED_FACE ( 'NONE', ( #11389 ), #9801, .F. ) ;
#2454 = LINE ( 'NONE', #812, #9672 ) ;
#2455 = CARTESIAN_POINT ( 'NONE',  ( -1.119409668803374558, 3.000000000000000000, -13.50845331674225669 ) ) ;
#2456 = CARTESIAN_POINT ( 'NONE',  ( 12.01285915242476499, 0.000000000000000000, -4.000000001073668265 ) ) ;
#2457 = VECTOR ( 'NONE', #2831, 1000.000000000000000 ) ;
#2458 = DIRECTION ( 'NONE',  ( 0.9254744032703045020, 0.000000000000000000, 0.3788101488760216018 ) ) ;
#2459 = CARTESIAN_POINT ( 'NONE',  ( 13.27898586450067242, 0.000000000000000000, -5.170206418547655502 ) ) ;
#2460 = ORIENTED_EDGE ( 'NONE', *, *, #12770, .F. ) ;
#2461 = ORIENTED_EDGE ( 'NONE', *, *, #3643, .F. ) ;
#2462 = VERTEX_POINT ( 'NONE', #13529 ) ;
#2463 = ORIENTED_EDGE ( 'NONE', *, *, #1910, .T. ) ;
#2464 = CARTESIAN_POINT ( 'NONE',  ( 12.37962962962963864, 3.000000000000000000, -12.43467921358330663 ) ) ;
#2465 = ADVANCED_FACE ( 'NONE', ( #9110 ), #13328, .T. ) ;
#2466 = ORIENTED_EDGE ( 'NONE', *, *, #7621, .F. ) ;
#2467 = CIRCLE ( 'NONE', #12394, 8.499999999999996447 ) ;
#2468 = CIRCLE ( 'NONE', #13473, 12.08999999999737440 ) ;
#2469 = CARTESIAN_POINT ( 'NONE',  ( -5.733772933379472470, 3.000000000000000000, 13.04554897075799502 ) ) ;
#2470 =( NAMED_UNIT ( * ) SI_UNIT ( $, .STERADIAN. ) SOLID_ANGLE_UNIT ( ) );
#2471 = B_SPLINE_SURFACE_WITH_KNOTS ( 'NONE', 3, 1, ( 
 ( #8433, #8498 ),
 ( #3851, #3981 ),
 ( #8116, #11365 ),
 ( #5018, #2958 ) ),
 .UNSPECIFIED., .F., .F., .F.,
 ( 4, 4 ),
 ( 2, 2 ),
 ( 0.7272709309819391787, 0.7566890080396341256 ),
 ( 0.000000000000000000, 1.000000000000000000 ),
 .UNSPECIFIED. ) ;
#2472 = EDGE_CURVE ( 'NONE', #3370, #11639, #1317, .T. ) ;
#2473 = CARTESIAN_POINT ( 'NONE',  ( -10.25006213149496936, 3.000000000000000000, -9.299128225235415712 ) ) ;
#2474 = CARTESIAN_POINT ( 'NONE',  ( 0.8327827707325454742, 9.000000000000000000, 6.698430626405788679 ) ) ;
#2475 = DIRECTION ( 'NONE',  ( -1.000000000000000000, 3.491481338843133355E-15, 2.602085213965210149E-16 ) ) ;
#2476 = CYLINDRICAL_SURFACE ( 'NONE', #4736, 1.000000000000000444 ) ;
#2477 = ORIENTED_EDGE ( 'NONE', *, *, #1478, .F. ) ;
#2478 = CARTESIAN_POINT ( 'NONE',  ( 31.00000000000000000, 3.000000000000000000, -1.073670993220974656E-09 ) ) ;
#2479 = AXIS2_PLACEMENT_3D ( 'NONE', #11242, #9024, #4832 ) ;
#2480 = ORIENTED_EDGE ( 'NONE', *, *, #6620, .F. ) ;
#2481 = ORIENTED_EDGE ( 'NONE', *, *, #3216, .T. ) ;
#2482 = CARTESIAN_POINT ( 'NONE',  ( -13.49999999999999645, 0.000000000000000000, -7.049999999999998934 ) ) ;
#2483 = EDGE_CURVE ( 'NONE', #3948, #9570, #10881, .T. ) ;
#2484 = EDGE_CURVE ( 'NONE', #8093, #9473, #8242, .T. ) ;
#2485 = ORIENTED_EDGE ( 'NONE', *, *, #264, .T. ) ;
#2486 = ORIENTED_EDGE ( 'NONE', *, *, #1201, .T. ) ;
#2487 = CARTESIAN_POINT ( 'NONE',  ( -8.352599575481690408, 0.000000000000000000, 30.99999999999999289 ) ) ;
#2488 = VECTOR ( 'NONE', #11981, 1000.000000000000000 ) ;
#2489 = FILL_AREA_STYLE ('',( #4555 ) ) ;
#2490 = CIRCLE ( 'NONE', #1626, 1.499999999999998668 ) ;
#2491 = CIRCLE ( 'NONE', #10190, 8.499999999999998224 ) ;
#2492 = DIRECTION ( 'NONE',  ( 0.000000000000000000, 1.000000000000000000, -0.000000000000000000 ) ) ;
#2493 = CARTESIAN_POINT ( 'NONE',  ( 0.8327827707325452522, 9.000000000000000000, 6.698430626405787791 ) ) ;
#2494 = AXIS2_PLACEMENT_3D ( 'NONE', #13026, #4690, #10061 ) ;
#2495 = CARTESIAN_POINT ( 'NONE',  ( -12.68816982652970893, 0.000000000000000000, 2.830255545554337004 ) ) ;
#2496 = CARTESIAN_POINT ( 'NONE',  ( -5.830003112347290184, 0.000000000000000000, -5.394061460138155795 ) ) ;
#2497 = CARTESIAN_POINT ( 'NONE',  ( 4.690415759823430619, 3.000000000000000000, -4.500000000000000888 ) ) ;
#2498 = EDGE_LOOP ( 'NONE', ( #9710, #6063, #1921, #7432 ) ) ;
#2499 = CARTESIAN_POINT ( 'NONE',  ( 3.007863545083557355, 9.000000000000000000, 7.350755164602351677 ) ) ;
#2500 = ORIENTED_EDGE ( 'NONE', *, *, #11734, .T. ) ;
#2501 = CIRCLE ( 'NONE', #8427, 6.750000000000000888 ) ;
#2502 = VERTEX_POINT ( 'NONE', #11794 ) ;
#2503 = VECTOR ( 'NONE', #6003, 1000.000000000000000 ) ;
#2504 = CIRCLE ( 'NONE', #4036, 14.25000000000000178 ) ;
#2505 = ORIENTED_EDGE ( 'NONE', *, *, #13043, .F. ) ;
#2506 = CARTESIAN_POINT ( 'NONE',  ( -0.8148820470561131124, 9.000000000000000000, 6.700631854488474204 ) ) ;
#2507 = CARTESIAN_POINT ( 'NONE',  ( 0.000000000000000000, 13.00000000000000178, 0.000000000000000000 ) ) ;
#2508 = CARTESIAN_POINT ( 'NONE',  ( 12.00000000000000888, 5.000000000000000000, -6.999999999999999112 ) ) ;
#2509 = CIRCLE ( 'NONE', #8877, 12.00000000000000000 ) ;
#2510 = CARTESIAN_POINT ( 'NONE',  ( 10.18987059060247269, 3.000000000000000000, 6.506507307819714647 ) ) ;
#2511 = AXIS2_PLACEMENT_3D ( 'NONE', #12551, #10542, #11313 ) ;
#2512 = FACE_OUTER_BOUND ( 'NONE', #7420, .T. ) ;
#2513 = CARTESIAN_POINT ( 'NONE',  ( 26.30958424017656938, 3.000000000000000000, 4.500000000000000888 ) ) ;
#2514 = CARTESIAN_POINT ( 'NONE',  ( -2.414978278956346092, 3.000000000000000000, 13.33788847341978467 ) ) ;
#2515 = ORIENTED_EDGE ( 'NONE', *, *, #2163, .T. ) ;
#2516 = EDGE_CURVE ( 'NONE', #1441, #816, #11183, .T. ) ;
#2517 = ORIENTED_EDGE ( 'NONE', *, *, #6588, .T. ) ;
#2518 = CIRCLE ( 'NONE', #8237, 1.500000000000000222 ) ;
#2519 = VECTOR ( 'NONE', #11293, 1000.000000000000000 ) ;
#2520 = VECTOR ( 'NONE', #3875, 1000.000000000000000 ) ;
#2521 = VERTEX_POINT ( 'NONE', #293 ) ;
#2522 = CARTESIAN_POINT ( 'NONE',  ( -8.914835885878215294, 3.000000000000000000, 11.11702303352197063 ) ) ;
#2523 = CARTESIAN_POINT ( 'NONE',  ( -6.017756925049793537, 3.000000000000000000, -11.52330688609026232 ) ) ;
#2524 = DIRECTION ( 'NONE',  ( 0.000000000000000000, 0.000000000000000000, 1.000000000000000000 ) ) ;
#2525 = CARTESIAN_POINT ( 'NONE',  ( 26.30958424017656938, 2.900000000000000355, 1.500000000000000000 ) ) ;
#2526 = CARTESIAN_POINT ( 'NONE',  ( -12.25282671965375236, 3.000000000000000000, 5.797378255456025364 ) ) ;
#2527 = STYLED_ITEM ( 'NONE', ( #7719 ), #3745 ) ;
#2528 = CARTESIAN_POINT ( 'NONE',  ( 6.951477219042924816, 9.000000000000000000, 3.842108769784387423 ) ) ;
#2529 = CIRCLE ( 'NONE', #8674, 1.500000000000001332 ) ;
#2530 = ADVANCED_FACE ( 'NONE', ( #11596 ), #2151, .F. ) ;
#2531 = DIRECTION ( 'NONE',  ( -0.000000000000000000, -1.000000000000000000, -0.000000000000000000 ) ) ;
#2532 = EDGE_CURVE ( 'NONE', #10516, #3746, #4067, .T. ) ;
#2533 = EDGE_LOOP ( 'NONE', ( #3440, #12296, #7097, #7171 ) ) ;
#2534 = ORIENTED_EDGE ( 'NONE', *, *, #6327, .F. ) ;
#2535 = ORIENTED_EDGE ( 'NONE', *, *, #458, .F. ) ;
#2536 = EDGE_LOOP ( 'NONE', ( #10265, #6533, #1609, #3765 ) ) ;
#2537 = CARTESIAN_POINT ( 'NONE',  ( -13.27898586450070084, 3.000000000000000000, -5.170206418547588001 ) ) ;
#2538 = EDGE_CURVE ( 'NONE', #11094, #10001, #5591, .T. ) ;
#2539 = ORIENTED_EDGE ( 'NONE', *, *, #13367, .F. ) ;
#2540 = COLOUR_RGB ( '',0.7803921568627451011, 0.7607843137254901578, 0.7411764705882353255 ) ;
#2541 = AXIS2_PLACEMENT_3D ( 'NONE', #9215, #7296, #13427 ) ;
#2542 = DIRECTION ( 'NONE',  ( -0.000000000000000000, -1.000000000000000000, -0.000000000000000000 ) ) ;
#2543 =( NAMED_UNIT ( * ) PLANE_ANGLE_UNIT ( ) SI_UNIT ( $, .RADIAN. ) );
#2544 = DIRECTION ( 'NONE',  ( 0.000000000000000000, 0.000000000000000000, 1.000000000000000000 ) ) ;
#2545 = CARTESIAN_POINT ( 'NONE',  ( -13.27898586450070084, 3.000000000000000000, -5.170206418547585336 ) ) ;
#2546 = CARTESIAN_POINT ( 'NONE',  ( 0.000000000000000000, 3.000000000000000000, -3.500000000000000888 ) ) ;
#2547 = EDGE_CURVE ( 'NONE', #2462, #13403, #13162, .T. ) ;
#2548 = DIRECTION ( 'NONE',  ( 0.000000000000000000, 0.000000000000000000, 1.000000000000000000 ) ) ;
#2549 = CARTESIAN_POINT ( 'NONE',  ( 2.428572470324196431, 0.000000000000000000, 13.33579367773357127 ) ) ;
#2550 = ORIENTED_EDGE ( 'NONE', *, *, #1716, .F. ) ;
#2551 = LINE ( 'NONE', #8373, #7050 ) ;
#2552 = CARTESIAN_POINT ( 'NONE',  ( 5.170206418547656391, 0.000000000000000000, 13.27898586450067064 ) ) ;
#2553 = ORIENTED_EDGE ( 'NONE', *, *, #10391, .F. ) ;
#2554 = EDGE_CURVE ( 'NONE', #9891, #9128, #4353, .T. ) ;
#2555 = ORIENTED_EDGE ( 'NONE', *, *, #8829, .F. ) ;
#2556 = CARTESIAN_POINT ( 'NONE',  ( 4.286263797015737088E-16, 2.900000000000000355, 3.500000000000000888 ) ) ;
#2557 = EDGE_CURVE ( 'NONE', #3424, #10069, #12758, .T. ) ;
#2558 = VERTEX_POINT ( 'NONE', #10693 ) ;
#2559 = ORIENTED_EDGE ( 'NONE', *, *, #10713, .F. ) ;
#2560 = CARTESIAN_POINT ( 'NONE',  ( 1.580708947611199511, 9.000000000000000000, -8.351727918397596540 ) ) ;
#2561 =( NAMED_UNIT ( * ) SI_UNIT ( $, .STERADIAN. ) SOLID_ANGLE_UNIT ( ) );
#2562 = CARTESIAN_POINT ( 'NONE',  ( -13.86115248177182835, 0.000000000000000000, -5.741477348071267528 ) ) ;
#2563 = CARTESIAN_POINT ( 'NONE',  ( 9.375397774054407662, 3.000000000000000000, -11.70905276178460497 ) ) ;
#2564 = CARTESIAN_POINT ( 'NONE',  ( 31.00000000000000000, 3.000000000000000000, 3.399999999999999911 ) ) ;
#2565 = CYLINDRICAL_SURFACE ( 'NONE', #2668, 12.08999999999737440 ) ;
#2566 = ADVANCED_FACE ( 'NONE', ( #2215 ), #5311, .T. ) ;
#2567 = DIRECTION ( 'NONE',  ( -0.000000000000000000, -1.000000000000000000, -0.000000000000000000 ) ) ;
#2568 = EDGE_LOOP ( 'NONE', ( #11980, #11539, #3859, #1127 ) ) ;
#2569 = DIRECTION ( 'NONE',  ( 0.000000000000000000, -1.000000000000000000, 0.000000000000000000 ) ) ;
#2570 = ORIENTED_EDGE ( 'NONE', *, *, #8684, .T. ) ;
#2571 = ORIENTED_EDGE ( 'NONE', *, *, #7250, .T. ) ;
#2572 = ORIENTED_EDGE ( 'NONE', *, *, #7675, .F. ) ;
#2573 = DIRECTION ( 'NONE',  ( -0.000000000000000000, -1.000000000000000000, -0.000000000000000000 ) ) ;
#2574 = FACE_OUTER_BOUND ( 'NONE', #10870, .T. ) ;
#2575 = PLANE ( 'NONE',  #10618 ) ;
#2576 = CARTESIAN_POINT ( 'NONE',  ( 26.30958424017656938, 3.000000000000000000, -1.500000000000000000 ) ) ;
#2577 = CARTESIAN_POINT ( 'NONE',  ( 1.836970198721030181E-16, 2.900000000000000355, 1.500000000000000222 ) ) ;
#2578 = EDGE_CURVE ( 'NONE', #3210, #5310, #5598, .T. ) ;
#2579 = CARTESIAN_POINT ( 'NONE',  ( 9.375397774054407662, 0.000000000000000000, -11.70905276178460497 ) ) ;
#2580 = DIRECTION ( 'NONE',  ( 0.000000000000000000, -1.000000000000000000, 0.000000000000000000 ) ) ;
#2581 = ADVANCED_FACE ( 'NONE', ( #226 ), #4945, .T. ) ;
#2582 = CARTESIAN_POINT ( 'NONE',  ( 2.631756770590782057, 3.000000000000000000, -14.20034848914875347 ) ) ;
#2583 = VERTEX_POINT ( 'NONE', #7455 ) ;
#2584 = ORIENTED_EDGE ( 'NONE', *, *, #8168, .F. ) ;
#2585 = B_SPLINE_SURFACE_WITH_KNOTS ( 'NONE', 3, 1, ( 
 ( #236, #6700 ),
 ( #12840, #2296 ),
 ( #11803, #2366 ),
 ( #4627, #12909 ) ),
 .UNSPECIFIED., .F., .F., .F.,
 ( 4, 4 ),
 ( 2, 2 ),
 ( 0.8181806201944104018, 0.8475986972523573693 ),
 ( 0.000000000000000000, 1.000000000000000000 ),
 .UNSPECIFIED. ) ;
#2586 = ORIENTED_EDGE ( 'NONE', *, *, #279, .T. ) ;
#2587 = CARTESIAN_POINT ( 'NONE',  ( 0.000000000000000000, 13.00000000000000178, 0.000000000000000000 ) ) ;
#2588 = DIRECTION ( 'NONE',  ( 0.000000000000000000, 1.000000000000000000, -0.000000000000000000 ) ) ;
#2589 = CARTESIAN_POINT ( 'NONE',  ( -11.52662650599083882, 3.000000000000000000, 3.647599401157695986 ) ) ;
#2590 = CARTESIAN_POINT ( 'NONE',  ( -8.158551673544545579, 3.000000000000000000, 8.922226997226644585 ) ) ;
#2591 = CARTESIAN_POINT ( 'NONE',  ( -2.264806262022998062, 3.000000000000000000, -14.82803603298499340 ) ) ;
#2592 = CYLINDRICAL_SURFACE ( 'NONE', #11322, 3.499999999999999556 ) ;
#2593 = CARTESIAN_POINT ( 'NONE',  ( 0.000000000000000000, 14.00000000000000178, -2.500000000000000000 ) ) ;
#2594 = CARTESIAN_POINT ( 'NONE',  ( -0.8148820470561131124, 9.000000000000000000, 6.700631854488474204 ) ) ;
#2595 = ORIENTED_EDGE ( 'NONE', *, *, #609, .T. ) ;
#2596 = ORIENTED_EDGE ( 'NONE', *, *, #4648, .T. ) ;
#2597 = ORIENTED_EDGE ( 'NONE', *, *, #10550, .F. ) ;
#2598 = CARTESIAN_POINT ( 'NONE',  ( 0.000000000000000000, 3.000000000000000000, 5.000000000000000000 ) ) ;
#2599 = EDGE_LOOP ( 'NONE', ( #6343, #179, #10416, #11865 ) ) ;
#2600 = EDGE_CURVE ( 'NONE', #4662, #1924, #12828, .T. ) ;
#2601 = CARTESIAN_POINT ( 'NONE',  ( 11.48836750521724070, 3.000000000000000000, 8.430890348300627224 ) ) ;
#2602 = SURFACE_STYLE_FILL_AREA ( #11988 ) ;
#2603 = DIRECTION ( 'NONE',  ( 0.000000000000000000, 1.000000000000000000, -0.000000000000000000 ) ) ;
#2604 = CARTESIAN_POINT ( 'NONE',  ( 5.967832595844252630, 9.000000000000000000, -3.153961652902406154 ) ) ;
#2605 = CARTESIAN_POINT ( 'NONE',  ( 3.061616997868383634E-16, 1.000000000000000000, 2.500000000000000444 ) ) ;
#2606 = CYLINDRICAL_SURFACE ( 'NONE', #3781, 14.25000000000000355 ) ;
#2607 = CARTESIAN_POINT ( 'NONE',  ( 2.604531154829233586, 0.000000000000000000, 11.80612203322752585 ) ) ;
#2608 = ORIENTED_EDGE ( 'NONE', *, *, #7398, .F. ) ;
#2609 = ORIENTED_EDGE ( 'NONE', *, *, #11038, .F. ) ;
#2610 = VERTEX_POINT ( 'NONE', #8403 ) ;
#2611 = DIRECTION ( 'NONE',  ( -0.000000000000000000, -1.000000000000000000, -0.000000000000000000 ) ) ;
#2612 = ORIENTED_EDGE ( 'NONE', *, *, #6570, .F. ) ;
#2613 = EDGE_CURVE ( 'NONE', #4963, #8964, #21, .T. ) ;
#2614 = ORIENTED_EDGE ( 'NONE', *, *, #2304, .T. ) ;
#2615 = EDGE_CURVE ( 'NONE', #11718, #9350, #5511, .T. ) ;
#2616 = DIRECTION ( 'NONE',  ( 0.000000000000000000, 1.000000000000000000, -0.000000000000000000 ) ) ;
#2617 = CARTESIAN_POINT ( 'NONE',  ( 45.60964950616533287, 3.000000000000000000, -15.50984893380129392 ) ) ;
#2618 = DIRECTION ( 'NONE',  ( 0.000000000000000000, 0.000000000000000000, 1.000000000000000000 ) ) ;
#2619 = EDGE_CURVE ( 'NONE', #11339, #10516, #1462, .T. ) ;
#2620 = CARTESIAN_POINT ( 'NONE',  ( -12.07793442604883971, 3.000000000000000000, 0.5400000000008015055 ) ) ;
#2621 = ADVANCED_FACE ( 'NONE', ( #9786 ), #1669, .F. ) ;
#2622 = LINE ( 'NONE', #3865, #12146 ) ;
#2623 = AXIS2_PLACEMENT_3D ( 'NONE', #3492, #10800, #11910 ) ;
#2624 = CARTESIAN_POINT ( 'NONE',  ( -6.025412986832177076, 3.000000000000000000, -13.73660796332610268 ) ) ;
#2625 = EDGE_LOOP ( 'NONE', ( #3351, #9646, #11379, #4240 ) ) ;
#2626 = CARTESIAN_POINT ( 'NONE',  ( 6.736042615721505200, 9.000000000000000000, 5.184180733653466433 ) ) ;
#2627 = ORIENTED_EDGE ( 'NONE', *, *, #10538, .T. ) ;
#2628 = ORIENTED_EDGE ( 'NONE', *, *, #12319, .T. ) ;
#2629 = ORIENTED_EDGE ( 'NONE', *, *, #7346, .F. ) ;
#2630 = ADVANCED_FACE ( 'NONE', ( #4766 ), #12004, .F. ) ;
#2631 = CARTESIAN_POINT ( 'NONE',  ( -14.39763212228013955, 3.000000000000000000, -1.133238802859595884 ) ) ;
#2632 = DIRECTION ( 'NONE',  ( 0.000000000000000000, 1.000000000000000000, 0.000000000000000000 ) ) ;
#2633 = FACE_OUTER_BOUND ( 'NONE', #5576, .T. ) ;
#2634 = CARTESIAN_POINT ( 'NONE',  ( -8.890701948131944476, 3.000000000000000000, 13.39999999999999858 ) ) ;
#2635 = CARTESIAN_POINT ( 'NONE',  ( 28.54655175640005282, 0.09999999999999982514, -2.353846153846154809 ) ) ;
#2636 = CARTESIAN_POINT ( 'NONE',  ( -6.025412986832177076, 3.000000000000000000, -13.73660796332610268 ) ) ;
#2637 = DIRECTION ( 'NONE',  ( 0.6923076923076927347, 1.270456495237146852E-16, 0.7216024245882196597 ) ) ;
#2638 = DIRECTION ( 'NONE',  ( -0.000000000000000000, -1.000000000000000000, -0.000000000000000000 ) ) ;
#2639 = B_SPLINE_CURVE_WITH_KNOTS ( 'NONE', 3,
 ( #8648, #11628, #1156, #4453 ),
 .UNSPECIFIED., .F., .F.,
 ( 4, 4 ),
 ( 0.1547128134717859205, 1.000000000000000000 ),
 .UNSPECIFIED. ) ;
#2640 = FACE_OUTER_BOUND ( 'NONE', #4685, .T. ) ;
#2641 = FACE_OUTER_BOUND ( 'NONE', #9845, .T. ) ;
#2642 = VECTOR ( 'NONE', #8013, 1000.000000000000000 ) ;
#2643 = AXIS2_PLACEMENT_3D ( 'NONE', #3715, #7791, #7918 ) ;
#2644 = ORIENTED_EDGE ( 'NONE', *, *, #2953, .F. ) ;
#2645 = VERTEX_POINT ( 'NONE', #9989 ) ;
#2646 = ADVANCED_FACE ( 'NONE', ( #5863 ), #3982, .F. ) ;
#2647 = ORIENTED_EDGE ( 'NONE', *, *, #13125, .T. ) ;
#2648 = CARTESIAN_POINT ( 'NONE',  ( 5.571433138827823761, 0.000000000000000000, 10.72973591378220704 ) ) ;
#2649 = DIRECTION ( 'NONE',  ( 0.000000000000000000, 0.000000000000000000, -1.000000000000000000 ) ) ;
#2650 = AXIS2_PLACEMENT_3D ( 'NONE', #8607, #12835, #1579 ) ;
#2651 = B_SPLINE_SURFACE_WITH_KNOTS ( 'NONE', 2, 1, ( 
 ( #8768, #7744 ),
 ( #1048, #2014 ),
 ( #2210, #9311 ) ),
 .UNSPECIFIED., .F., .F., .F.,
 ( 3, 3 ),
 ( 2, 2 ),
 ( 0.000000000000000000, 1.000000000000000000 ),
 ( 0.000000000000000000, 1.000000000000000000 ),
 .UNSPECIFIED. ) ;
#2652 = VECTOR ( 'NONE', #7773, 1000.000000000000000 ) ;
#2653 = DIRECTION ( 'NONE',  ( 0.000000000000000000, 1.000000000000000000, 0.000000000000000000 ) ) ;
#2654 = DIRECTION ( 'NONE',  ( -0.000000000000000000, -1.000000000000000000, -0.000000000000000000 ) ) ;
#2655 = CARTESIAN_POINT ( 'NONE',  ( -20.56403552112892896, 3.000000000000000000, -16.70078978407140013 ) ) ;
#2656 = CARTESIAN_POINT ( 'NONE',  ( 5.985774866078161338, 0.000000000000000000, 3.119775513178307147 ) ) ;
#2657 = CYLINDRICAL_SURFACE ( 'NONE', #3605, 14.24999999999999822 ) ;
#2658 = CARTESIAN_POINT ( 'NONE',  ( 3.000000000000001776, 2.000000000000000000, 10.00000000000000000 ) ) ;
#2659 = VERTEX_POINT ( 'NONE', #7789 ) ;
#2660 = AXIS2_PLACEMENT_3D ( 'NONE', #9121, #8907, #11125 ) ;
#2661 = ORIENTED_EDGE ( 'NONE', *, *, #2022, .T. ) ;
#2662 = VECTOR ( 'NONE', #2711, 1000.000000000000000 ) ;
#2663 = ORIENTED_EDGE ( 'NONE', *, *, #271, .F. ) ;
#2664 = CARTESIAN_POINT ( 'NONE',  ( 31.00000000000000000, 0.09999999999999982514, -3.499999999999999556 ) ) ;
#2665 = VERTEX_POINT ( 'NONE', #6816 ) ;
#2666 = CARTESIAN_POINT ( 'NONE',  ( 9.573149624528804580, 0.000000000000000000, -8.795158114916638681 ) ) ;
#2667 = DIRECTION ( 'NONE',  ( -0.8355447873043153617, -8.902706987485325619E-16, -0.5494223406529682441 ) ) ;
#2668 = AXIS2_PLACEMENT_3D ( 'NONE', #2766, #13314, #8888 ) ;
#2669 = EDGE_CURVE ( 'NONE', #7043, #2208, #93, .T. ) ;
#2670 = DIRECTION ( 'NONE',  ( -2.312964634635742267E-15, 0.000000000000000000, 1.000000000000000000 ) ) ;
#2671 = CARTESIAN_POINT ( 'NONE',  ( -6.057461899949976747, 0.000000000000000000, 5.137313564148215939 ) ) ;
#2672 = CARTESIAN_POINT ( 'NONE',  ( -7.125870497355421662, 9.000000000000000000, -3.507536778237742237 ) ) ;
#2673 = DIRECTION ( 'NONE',  ( -0.000000000000000000, -1.000000000000000000, -0.000000000000000000 ) ) ;
#2674 = CARTESIAN_POINT ( 'NONE',  ( 7.499999999999999112, 0.000000000000000000, 0.000000000000000000 ) ) ;
#2675 = ORIENTED_EDGE ( 'NONE', *, *, #2310, .F. ) ;
#2676 = PRESENTATION_STYLE_ASSIGNMENT (( #13155 ) ) ;
#2677 = VERTEX_POINT ( 'NONE', #5711 ) ;
#2678 = EDGE_CURVE ( 'NONE', #4801, #9824, #12623, .T. ) ;
#2679 = VECTOR ( 'NONE', #11755, 1000.000000000000000 ) ;
#2680 = ORIENTED_EDGE ( 'NONE', *, *, #6184, .T. ) ;
#2681 = CARTESIAN_POINT ( 'NONE',  ( -5.170206418547658167, 3.000000000000000000, -13.27898586450066887 ) ) ;
#2682 = VERTEX_POINT ( 'NONE', #2487 ) ;
#2683 = CARTESIAN_POINT ( 'NONE',  ( 0.000000000000000000, 0.000000000000000000, 0.000000000000000000 ) ) ;
#2684 = ORIENTED_EDGE ( 'NONE', *, *, #2047, .T. ) ;
#2685 = CARTESIAN_POINT ( 'NONE',  ( -12.30759122141990325, 0.000000000000000000, -6.329356821613475681 ) ) ;
#2686 =( NAMED_UNIT ( * ) SI_UNIT ( $, .STERADIAN. ) SOLID_ANGLE_UNIT ( ) );
#2687 = CARTESIAN_POINT ( 'NONE',  ( -6.025412986832177076, 0.000000000000000000, -13.73660796332610268 ) ) ;
#2688 = AXIS2_PLACEMENT_3D ( 'NONE', #1186, #4141, #4204 ) ;
#2689 = FACE_OUTER_BOUND ( 'NONE', #5970, .T. ) ;
#2690 = VECTOR ( 'NONE', #10705, 1000.000000000000000 ) ;
#2691 = DIRECTION ( 'NONE',  ( -0.9100336346413742117, -0.000000000000000000, -0.4145344181384821858 ) ) ;
#2692 = PLANE ( 'NONE',  #4507 ) ;
#2693 = VERTEX_POINT ( 'NONE', #12900 ) ;
#2694 = FACE_BOUND ( 'NONE', #2698, .T. ) ;
#2695 = ADVANCED_FACE ( 'NONE', ( #8882 ), #3711, .T. ) ;
#2696 = ORIENTED_EDGE ( 'NONE', *, *, #3385, .T. ) ;
#2697 = EDGE_CURVE ( 'NONE', #9762, #10809, #4786, .T. ) ;
#2698 = EDGE_LOOP ( 'NONE', ( #8476, #417 ) ) ;
#2699 = DIRECTION ( 'NONE',  ( -0.000000000000000000, -1.000000000000000000, -0.000000000000000000 ) ) ;
#2700 = ORIENTED_EDGE ( 'NONE', *, *, #7210, .T. ) ;
#2701 = VECTOR ( 'NONE', #12682, 1000.000000000000000 ) ;
#2702 = AXIS2_PLACEMENT_3D ( 'NONE', #12467, #3258, #1071 ) ;
#2703 = EDGE_CURVE ( 'NONE', #933, #7402, #11531, .T. ) ;
#2704 = DIRECTION ( 'NONE',  ( 0.000000000000000000, 0.000000000000000000, -1.000000000000000000 ) ) ;
#2705 = DIRECTION ( 'NONE',  ( 0.000000000000000000, 1.000000000000000000, 0.000000000000000000 ) ) ;
#2706 = CYLINDRICAL_SURFACE ( 'NONE', #3561, 1.500000000000000222 ) ;
#2707 = DIRECTION ( 'NONE',  ( 0.000000000000000000, 0.000000000000000000, -1.000000000000000000 ) ) ;
#2708 = CARTESIAN_POINT ( 'NONE',  ( -1.133238802859761973, 3.000000000000000000, -14.39763212228013067 ) ) ;
#2709 = CONTEXT_DEPENDENT_SHAPE_REPRESENTATION ( #4667, #2164 ) ;
#2710 = DIRECTION ( 'NONE',  ( 0.000000000000000000, 1.000000000000000000, 0.000000000000000000 ) ) ;
#2711 = DIRECTION ( 'NONE',  ( -0.000000000000000000, -1.000000000000000000, -0.000000000000000000 ) ) ;
#2712 = FACE_BOUND ( 'NONE', #10036, .T. ) ;
#2713 = VECTOR ( 'NONE', #1904, 1000.000000000000000 ) ;
#2714 = LINE ( 'NONE', #11189, #4255 ) ;
#2715 = DIRECTION ( 'NONE',  ( -0.000000000000000000, -1.000000000000000000, -0.000000000000000000 ) ) ;
#2716 = CIRCLE ( 'NONE', #12192, 14.25000000000000178 ) ;
#2717 = CIRCLE ( 'NONE', #1627, 1.500000000000003997 ) ;
#2718 = ADVANCED_FACE ( 'NONE', ( #11928 ), #365, .T. ) ;
#2719 = ORIENTED_EDGE ( 'NONE', *, *, #3807, .T. ) ;
#2720 = CIRCLE ( 'NONE', #5368, 13.50000000000000178 ) ;
#2721 = ORIENTED_EDGE ( 'NONE', *, *, #4452, .F. ) ;
#2722 = ADVANCED_FACE ( 'NONE', ( #1593 ), #1915, .F. ) ;
#2723 = ORIENTED_EDGE ( 'NONE', *, *, #13134, .F. ) ;
#2724 = CARTESIAN_POINT ( 'NONE',  ( 5.731782959214990036, 3.000000000000000000, 11.46814821560793618 ) ) ;
#2725 = AXIS2_PLACEMENT_3D ( 'NONE', #3495, #5496, #8730 ) ;
#2726 = CARTESIAN_POINT ( 'NONE',  ( 7.723663868796767140, 0.000000000000000000, 11.13895890373327191 ) ) ;
#2727 = CYLINDRICAL_SURFACE ( 'NONE', #10629, 1.500000000000000222 ) ;
#2728 = DIRECTION ( 'NONE',  ( 0.000000000000000000, 0.000000000000000000, 1.000000000000000000 ) ) ;
#2729 = CARTESIAN_POINT ( 'NONE',  ( -8.430890348300124515, 3.000000000000000000, 11.48836750521761019 ) ) ;
#2730 = FACE_OUTER_BOUND ( 'NONE', #10027, .T. ) ;
#2731 = EDGE_CURVE ( 'NONE', #10022, #7906, #2369, .T. ) ;
#2732 = CARTESIAN_POINT ( 'NONE',  ( 2.830255545554135832, 3.000000000000000000, -12.68816982652952596 ) ) ;
#2733 = EDGE_CURVE ( 'NONE', #10192, #8876, #5097, .T. ) ;
#2734 = VECTOR ( 'NONE', #1978, 1000.000000000000000 ) ;
#2735 = CARTESIAN_POINT ( 'NONE',  ( 10.00000000000001243, 5.000000000000007105, 7.000000000000001776 ) ) ;
#2736 = AXIS2_PLACEMENT_3D ( 'NONE', #3850, #9073, #8050 ) ;
#2737 = VERTEX_POINT ( 'NONE', #12491 ) ;
#2738 = ORIENTED_EDGE ( 'NONE', *, *, #2678, .F. ) ;
#2739 = ORIENTED_EDGE ( 'NONE', *, *, #12101, .F. ) ;
#2740 = CARTESIAN_POINT ( 'NONE',  ( 0.5501230721522984979, 0.000000000000000000, -12.98835496148321766 ) ) ;
#2741 = APPLICATION_CONTEXT ( 'automotive_design' ) ;
#2742 = EDGE_LOOP ( 'NONE', ( #7316, #3855, #5293, #2942 ) ) ;
#2743 = CARTESIAN_POINT ( 'NONE',  ( -2.428572470324203980, 3.000000000000000000, -13.33579367773357482 ) ) ;
#2744 = AXIS2_PLACEMENT_3D ( 'NONE', #13045, #3525, #3664 ) ;
#2745 = DIRECTION ( 'NONE',  ( 1.000000000000000000, 0.000000000000000000, 0.000000000000000000 ) ) ;
#2746 = CIRCLE ( 'NONE', #11333, 6.750000000000000888 ) ;
#2747 = CARTESIAN_POINT ( 'NONE',  ( 1.557181465540669496, 0.000000000000000000, -14.16466328168010769 ) ) ;
#2748 = DIRECTION ( 'NONE',  ( 0.000000000000000000, 1.000000000000000000, 0.000000000000000000 ) ) ;
#2749 = LINE ( 'NONE', #13292, #4500 ) ;
#2750 = DIRECTION ( 'NONE',  ( -1.000000000000000000, 0.000000000000000000, 0.000000000000000000 ) ) ;
#2751 = CARTESIAN_POINT ( 'NONE',  ( 53.04054522416362261, 0.000000000000000000, -3.611077387296437013 ) ) ;
#2752 = EDGE_CURVE ( 'NONE', #4632, #5256, #3472, .T. ) ;
#2753 = ORIENTED_EDGE ( 'NONE', *, *, #10720, .T. ) ;
#2754 = CARTESIAN_POINT ( 'NONE',  ( -5.571433138827826426, 3.000000000000000000, -10.72973591378220526 ) ) ;
#2755 = VERTEX_POINT ( 'NONE', #900 ) ;
#2756 = VECTOR ( 'NONE', #1118, 1000.000000000000000 ) ;
#2757 = ORIENTED_EDGE ( 'NONE', *, *, #4870, .T. ) ;
#2758 = CARTESIAN_POINT ( 'NONE',  ( -7.798201703419555209, 0.000000000000000000, -30.99999999999999289 ) ) ;
#2759 = EDGE_LOOP ( 'NONE', ( #4791, #11244, #3057, #10602 ) ) ;
#2760 = CARTESIAN_POINT ( 'NONE',  ( 7.500000000000003553, 0.000000000000000000, 13.39999999999999858 ) ) ;
#2761 = ORIENTED_EDGE ( 'NONE', *, *, #949, .T. ) ;
#2762 = CARTESIAN_POINT ( 'NONE',  ( 0.000000000000000000, 3.000000000000000000, 0.000000000000000000 ) ) ;
#2763 = CARTESIAN_POINT ( 'NONE',  ( 0.000000000000000000, 14.00000000000000178, 0.000000000000000000 ) ) ;
#2764 =( GEOMETRIC_REPRESENTATION_CONTEXT ( 3 ) GLOBAL_UNCERTAINTY_ASSIGNED_CONTEXT ( ( #8059 ) ) GLOBAL_UNIT_ASSIGNED_CONTEXT ( ( #9635, #6539, #2470 ) ) REPRESENTATION_CONTEXT ( 'NONE', 'WORKASPACE' ) );
#2765 = CARTESIAN_POINT ( 'NONE',  ( 9.573149624528804580, 0.000000000000000000, -8.795158114916638681 ) ) ;
#2766 = CARTESIAN_POINT ( 'NONE',  ( 0.000000000000000000, 3.000000000000000000, 0.000000000000000000 ) ) ;
#2767 = DIRECTION ( 'NONE',  ( 1.000000000000000000, 0.000000000000000000, 1.224646799147353207E-16 ) ) ;
#2768 = ORIENTED_EDGE ( 'NONE', *, *, #4568, .F. ) ;
#2769 = CARTESIAN_POINT ( 'NONE',  ( -13.49999999999999645, 3.000000000000000000, -7.049999999999998934 ) ) ;
#2770 = ORIENTED_EDGE ( 'NONE', *, *, #8658, .T. ) ;
#2771 = EDGE_LOOP ( 'NONE', ( #2209, #11836, #4445, #10124 ) ) ;
#2772 = CARTESIAN_POINT ( 'NONE',  ( 7.151505841916629080, -1.694065894508600678E-18, 1.752496229622501511 ) ) ;
#2773 = B_SPLINE_SURFACE_WITH_KNOTS ( 'NONE', 3, 1, ( 
 ( #8089, #6847 ),
 ( #11049, #8019 ),
 ( #10016, #4848 ),
 ( #12240, #13338 ) ),
 .UNSPECIFIED., .F., .F., .F.,
 ( 4, 4 ),
 ( 2, 2 ),
 ( 0.1547128134717859205, 1.000000000000000000 ),
 ( 0.000000000000000000, 1.000000000000000000 ),
 .UNSPECIFIED. ) ;
#2774 = ORIENTED_EDGE ( 'NONE', *, *, #7448, .T. ) ;
#2775 = DIRECTION ( 'NONE',  ( -0.000000000000000000, -1.000000000000000000, -0.000000000000000000 ) ) ;
#2776 = DIRECTION ( 'NONE',  ( 1.000000000000000000, 0.000000000000000000, 0.000000000000000000 ) ) ;
#2777 = LINE ( 'NONE', #11117, #4290 ) ;
#2778 = CARTESIAN_POINT ( 'NONE',  ( 0.000000000000000000, 0.000000000000000000, 0.000000000000000000 ) ) ;
#2779 = CARTESIAN_POINT ( 'NONE',  ( 7.110882674384088276, 9.000000000000000000, -3.538387050178523729 ) ) ;
#2780 = EDGE_CURVE ( 'NONE', #13316, #10663, #7108, .T. ) ;
#2781 = DIRECTION ( 'NONE',  ( 0.7216024245882196597, 0.000000000000000000, 0.6923076923076926237 ) ) ;
#2782 = DIRECTION ( 'NONE',  ( 0.000000000000000000, 0.000000000000000000, 1.000000000000000000 ) ) ;
#2783 = CARTESIAN_POINT ( 'NONE',  ( -3.833392836528145331, 1.734723475976807094E-15, -5.555861711818853799 ) ) ;
#2784 = CARTESIAN_POINT ( 'NONE',  ( 29.02231267299996986, 3.000000000000000000, -1.321950885510182250 ) ) ;
#2785 = CARTESIAN_POINT ( 'NONE',  ( -0.7901945867173586491, 0.000000000000000000, -12.78643498603818074 ) ) ;
#2786 = CARTESIAN_POINT ( 'NONE',  ( -7.363095878837111030, 9.000000000000000000, 0.009895496992605581216 ) ) ;
#2787 = ORIENTED_EDGE ( 'NONE', *, *, #9935, .F. ) ;
#2788 = ORIENTED_EDGE ( 'NONE', *, *, #9212, .T. ) ;
#2789 = ORIENTED_EDGE ( 'NONE', *, *, #1829, .F. ) ;
#2790 = VERTEX_POINT ( 'NONE', #10330 ) ;
#2791 = CARTESIAN_POINT ( 'NONE',  ( -8.482622935103766082, 0.000000000000000000, 9.600126836553263487 ) ) ;
#2792 = DIRECTION ( 'NONE',  ( 0.000000000000000000, 1.000000000000000000, -0.000000000000000000 ) ) ;
#2793 = EDGE_CURVE ( 'NONE', #4332, #9873, #11627, .T. ) ;
#2794 = CARTESIAN_POINT ( 'NONE',  ( -14.87484884897975057, 0.000000000000000000, 1.958311002203303453 ) ) ;
#2795 = DIRECTION ( 'NONE',  ( 0.000000000000000000, 1.000000000000000000, -0.000000000000000000 ) ) ;
#2796 = CARTESIAN_POINT ( 'NONE',  ( 5.733772933379453818, 3.000000000000000000, 13.04554897075800568 ) ) ;
#2797 = ADVANCED_FACE ( 'NONE', ( #10200 ), #2001, .T. ) ;
#2798 = CARTESIAN_POINT ( 'NONE',  ( 0.000000000000000000, -3.000000000000000000, 9.250000000000000000 ) ) ;
#2799 = EDGE_CURVE ( 'NONE', #12697, #9707, #6912, .T. ) ;
#2800 = CARTESIAN_POINT ( 'NONE',  ( 19.44487669093179605, 3.000000000000000000, -16.66326752702930847 ) ) ;
#2801 = DIRECTION ( 'NONE',  ( 0.000000000000000000, 0.000000000000000000, 1.000000000000000000 ) ) ;
#2802 = ORIENTED_EDGE ( 'NONE', *, *, #2554, .T. ) ;
#2803 = EDGE_LOOP ( 'NONE', ( #5343, #13058, #2787, #6487 ) ) ;
#2804 = ORIENTED_EDGE ( 'NONE', *, *, #12721, .F. ) ;
#2805 = CARTESIAN_POINT ( 'NONE',  ( 2.264806262022877714, 0.000000000000000000, -14.82803603298501471 ) ) ;
#2806 = ORIENTED_EDGE ( 'NONE', *, *, #11223, .F. ) ;
#2807 = CARTESIAN_POINT ( 'NONE',  ( -10.25006213149496936, 0.000000000000000000, -9.299128225235415712 ) ) ;
#2808 = DIRECTION ( 'NONE',  ( -0.7047873421805881389, 5.358158289871356379E-26, 0.7094186368442984003 ) ) ;
#2809 = CARTESIAN_POINT ( 'NONE',  ( 0.7901945867173618687, 3.000000000000000000, 12.78643498603817541 ) ) ;
#2810 = CARTESIAN_POINT ( 'NONE',  ( -0.8123631076467130452, 1.734723475976807094E-15, -6.700937709107178009 ) ) ;
#2811 = DIRECTION ( 'NONE',  ( 0.000000000000000000, 1.000000000000000000, -0.000000000000000000 ) ) ;
#2812 = CARTESIAN_POINT ( 'NONE',  ( -8.771102293099080072, 3.000000000000000000, -10.33484986938307770 ) ) ;
#2813 = DIRECTION ( 'NONE',  ( 1.000000000000000000, 0.000000000000000000, 1.224646799147353207E-16 ) ) ;
#2814 = EDGE_LOOP ( 'NONE', ( #5377, #501, #8859, #385 ) ) ;
#2815 = LINE ( 'NONE', #11015, #5780 ) ;
#2816 = APPLICATION_CONTEXT ( 'automotive_design' ) ;
#2817 = ORIENTED_EDGE ( 'NONE', *, *, #2379, .T. ) ;
#2818 = PRODUCT_DEFINITION_CONTEXT ( 'detailed design', #5544, 'design' ) ;
#2819 = ORIENTED_EDGE ( 'NONE', *, *, #12994, .T. ) ;
#2820 = CARTESIAN_POINT ( 'NONE',  ( -5.452638258930639914, 0.000000000000000000, -13.97385902380748313 ) ) ;
#2821 = ORIENTED_EDGE ( 'NONE', *, *, #10476, .F. ) ;
#2822 = CARTESIAN_POINT ( 'NONE',  ( -10.69794375946289655, 0.000000000000000000, -7.065816209474156118 ) ) ;
#2823 = EDGE_CURVE ( 'NONE', #6054, #3238, #1966, .T. ) ;
#2824 = ORIENTED_EDGE ( 'NONE', *, *, #4997, .F. ) ;
#2825 = EDGE_CURVE ( 'NONE', #5427, #12707, #3934, .T. ) ;
#2826 = CARTESIAN_POINT ( 'NONE',  ( 51.41686768994642165, 3.000000000000000000, -11.86457109001525545 ) ) ;
#2827 = CARTESIAN_POINT ( 'NONE',  ( -6.343077614891082128, 0.000000000000000000, -11.35348748332310720 ) ) ;
#2828 = FACE_OUTER_BOUND ( 'NONE', #6907, .T. ) ;
#2829 = B_SPLINE_CURVE_WITH_KNOTS ( 'NONE', 3,
 ( #723, #7871, #4919, #2783 ),
 .UNSPECIFIED., .F., .F.,
 ( 4, 4 ),
 ( 0.1276832474596281686, 1.000000000000000000 ),
 .UNSPECIFIED. ) ;
#2830 = DIRECTION ( 'NONE',  ( -0.000000000000000000, -1.000000000000000000, -0.000000000000000000 ) ) ;
#2831 = DIRECTION ( 'NONE',  ( -0.000000000000000000, -1.000000000000000000, -0.000000000000000000 ) ) ;
#2832 = CARTESIAN_POINT ( 'NONE',  ( -0.5400000000008023937, 0.000000000000000000, -12.07793442604883971 ) ) ;
#2833 = EDGE_LOOP ( 'NONE', ( #9784, #11805, #7652, #9155 ) ) ;
#2834 = CARTESIAN_POINT ( 'NONE',  ( 26.30958424017656938, 2.900000000000000355, -1.399999999999999911 ) ) ;
#2835 = ORIENTED_EDGE ( 'NONE', *, *, #9258, .T. ) ;
#2836 = EDGE_LOOP ( 'NONE', ( #12806, #8634, #12442, #5287 ) ) ;
#2837 = DIRECTION ( 'NONE',  ( 0.000000000000000000, 0.000000000000000000, -1.000000000000000000 ) ) ;
#2838 = B_SPLINE_CURVE_WITH_KNOTS ( 'NONE', 3,
 ( #3780, #5992, #9160, #6067 ),
 .UNSPECIFIED., .F., .F.,
 ( 4, 4 ),
 ( 0.000000000000000000, 0.5855695330273008592 ),
 .UNSPECIFIED. ) ;
#2839 = ORIENTED_EDGE ( 'NONE', *, *, #12497, .T. ) ;
#2840 = CARTESIAN_POINT ( 'NONE',  ( 8.504652361247167391, 3.000000000000000000, 9.593885948927674434 ) ) ;
#2841 = CARTESIAN_POINT ( 'NONE',  ( 10.33484986938308481, 0.000000000000000000, -8.771102293099065861 ) ) ;
#2842 = DIRECTION ( 'NONE',  ( 0.000000000000000000, 1.000000000000000000, -0.000000000000000000 ) ) ;
#2843 = CYLINDRICAL_SURFACE ( 'NONE', #4838, 4.000000000000000000 ) ;
#2844 = DIRECTION ( 'NONE',  ( 0.000000000000000000, 0.000000000000000000, 1.000000000000000000 ) ) ;
#2845 = CONTEXT_DEPENDENT_SHAPE_REPRESENTATION ( #6086, #9748 ) ;
#2846 = CARTESIAN_POINT ( 'NONE',  ( -9.324917476840782982, 0.000000000000000000, -9.065441278446241924 ) ) ;
#2847 = DIRECTION ( 'NONE',  ( 0.000000000000000000, 1.000000000000000000, 0.000000000000000000 ) ) ;
#2848 = CARTESIAN_POINT ( 'NONE',  ( 5.733772933379453818, 3.000000000000000000, 13.04554897075800568 ) ) ;
#2849 = DIRECTION ( 'NONE',  ( 0.6291930273682743158, 0.000000000000000000, -0.7772490812546168915 ) ) ;
#2850 = CARTESIAN_POINT ( 'NONE',  ( -4.072642252455976219, 3.000000000000000000, -12.14623037080101398 ) ) ;
#2851 = VERTEX_POINT ( 'NONE', #2894 ) ;
#2852 = VERTEX_POINT ( 'NONE', #2969 ) ;
#2853 = CIRCLE ( 'NONE', #8342, 14.25000000000000355 ) ;
#2854 = ADVANCED_FACE ( 'NONE', ( #3860 ), #262, .T. ) ;
#2855 = ORIENTED_EDGE ( 'NONE', *, *, #7920, .T. ) ;
#2856 = ORIENTED_EDGE ( 'NONE', *, *, #10469, .T. ) ;
#2857 = FACE_OUTER_BOUND ( 'NONE', #2771, .T. ) ;
#2858 = DIRECTION ( 'NONE',  ( -0.000000000000000000, -0.000000000000000000, -1.000000000000000000 ) ) ;
#2859 = FACE_OUTER_BOUND ( 'NONE', #3174, .T. ) ;
#2860 = AXIS2_PLACEMENT_3D ( 'NONE', #11334, #13183, #13336 ) ;
#2861 = CARTESIAN_POINT ( 'NONE',  ( 22.00000000000000000, 3.000000000000000000, 0.000000000000000000 ) ) ;
#2862 = CARTESIAN_POINT ( 'NONE',  ( 5.504794476853524188, -1.694065894508600678E-18, -4.890042597913815570 ) ) ;
#2863 = AXIS2_PLACEMENT_3D ( 'NONE', #6557, #4493, #2419 ) ;
#2864 = PLANE ( 'NONE',  #6038 ) ;
#2865 = CARTESIAN_POINT ( 'NONE',  ( 24.82664254338761722, 3.000000000000000000, 4.561072489069574409 ) ) ;
#2866 = ORIENTED_EDGE ( 'NONE', *, *, #2906, .T. ) ;
#2867 = EDGE_CURVE ( 'NONE', #12707, #5427, #12317, .T. ) ;
#2868 = CARTESIAN_POINT ( 'NONE',  ( 0.000000000000000000, -3.000000000000000000, 0.000000000000000000 ) ) ;
#2869 = ADVANCED_FACE ( 'NONE', ( #3030 ), #12352, .T. ) ;
#2870 = CARTESIAN_POINT ( 'NONE',  ( 0.1834774187694905023, 3.000000000000000000, -13.00394734430440025 ) ) ;
#2871 = PRESENTATION_LAYER_ASSIGNMENT (  '', '', ( #6386 ) ) ;
#2872 = ORIENTED_EDGE ( 'NONE', *, *, #12332, .F. ) ;
#2873 = ADVANCED_FACE ( 'NONE', ( #11165 ), #5327, .T. ) ;
#2874 = EDGE_CURVE ( 'NONE', #2852, #7906, #9163, .T. ) ;
#2875 = CARTESIAN_POINT ( 'NONE',  ( 31.00000000000000000, 0.000000000000000000, 3.399999999999999911 ) ) ;
#2876 = DIRECTION ( 'NONE',  ( -0.9353363873783847593, -6.543406766095367948E-22, 0.3537595828326807190 ) ) ;
#2877 = DIRECTION ( 'NONE',  ( -0.000000000000000000, -1.000000000000000000, -0.000000000000000000 ) ) ;
#2878 = CARTESIAN_POINT ( 'NONE',  ( 0.000000000000000000, 9.000000000000000000, 0.000000000000000000 ) ) ;
#2879 = DIRECTION ( 'NONE',  ( -1.000000000000000000, 3.469446951953610639E-15, 2.602085213965210149E-16 ) ) ;
#2880 = CIRCLE ( 'NONE', #10802, 1.500000000000000666 ) ;
#2881 = CARTESIAN_POINT ( 'NONE',  ( 0.000000000000000000, 3.000000000000000000, 0.000000000000000000 ) ) ;
#2882 = AXIS2_PLACEMENT_3D ( 'NONE', #2248, #1226, #11762 ) ;
#2883 = CARTESIAN_POINT ( 'NONE',  ( -13.52637830886122572, 0.000000000000000000, -2.928250210355275218 ) ) ;
#2884 = ORIENTED_EDGE ( 'NONE', *, *, #8769, .F. ) ;
#2885 = DIRECTION ( 'NONE',  ( -0.000000000000000000, -1.000000000000000000, -0.000000000000000000 ) ) ;
#2886 = EDGE_CURVE ( 'NONE', #2239, #2099, #3058, .T. ) ;
#2887 = ORIENTED_EDGE ( 'NONE', *, *, #3513, .T. ) ;
#2888 = EDGE_LOOP ( 'NONE', ( #9425, #10381, #6325, #10905 ) ) ;
#2889 = EDGE_LOOP ( 'NONE', ( #670, #6294, #3626, #6967 ) ) ;
#2890 = CARTESIAN_POINT ( 'NONE',  ( -14.82803603298502360, 3.000000000000000000, -2.264806262022826644 ) ) ;
#2891 = VERTEX_POINT ( 'NONE', #13375 ) ;
#2892 = EDGE_CURVE ( 'NONE', #6179, #5887, #11232, .T. ) ;
#2893 = AXIS2_PLACEMENT_3D ( 'NONE', #5033, #9229, #3233 ) ;
#2894 = CARTESIAN_POINT ( 'NONE',  ( -8.914835885878215294, 3.000000000000000000, 11.11702303352197063 ) ) ;
#2895 = FILL_AREA_STYLE ('',( #1938 ) ) ;
#2896 = CARTESIAN_POINT ( 'NONE',  ( 12.00000000000002309, 8.000000000000000000, 7.000000000000000888 ) ) ;
#2897 = CARTESIAN_POINT ( 'NONE',  ( -2.590203375110137873, 0.000000000000000000, 6.893050072893555758 ) ) ;
#2898 = B_SPLINE_CURVE_WITH_KNOTS ( 'NONE', 3,
 ( #13071, #1566, #11070, #3553 ),
 .UNSPECIFIED., .F., .F.,
 ( 4, 4 ),
 ( 0.000000000000000000, 0.5855695330273008592 ),
 .UNSPECIFIED. ) ;
#2899 = CARTESIAN_POINT ( 'NONE',  ( 0.000000000000000000, 9.000000000000000000, 0.000000000000000000 ) ) ;
#2900 = CARTESIAN_POINT ( 'NONE',  ( -13.27898586450070084, 3.000000000000000000, -5.170206418547588001 ) ) ;
#2901 = FACE_OUTER_BOUND ( 'NONE', #7066, .T. ) ;
#2902 = ORIENTED_EDGE ( 'NONE', *, *, #5723, .T. ) ;
#2903 = CIRCLE ( 'NONE', #7525, 1.600000000000004086 ) ;
#2904 = CARTESIAN_POINT ( 'NONE',  ( 2.161962830978694683, 0.000000000000000000, -14.08504230442587790 ) ) ;
#2905 = TOROIDAL_SURFACE ( 'NONE', #8819, 3.400000000000001243, 0.1000000000000000056 ) ;
#2906 = EDGE_CURVE ( 'NONE', #4948, #11926, #4310, .T. ) ;
#2907 = ORIENTED_EDGE ( 'NONE', *, *, #6482, .F. ) ;
#2908 = ADVANCED_FACE ( 'NONE', ( #12743, #1167, #6393, #150, #4399, #8460, #9, #12685, #2073, #5294 ), #7571, .T. ) ;
#2909 = ORIENTED_EDGE ( 'NONE', *, *, #5373, .T. ) ;
#2910 = CARTESIAN_POINT ( 'NONE',  ( -11.80615107470192804, 3.000000000000000000, -2.604399508764160487 ) ) ;
#2911 = ORIENTED_EDGE ( 'NONE', *, *, #13125, .F. ) ;
#2912 = CARTESIAN_POINT ( 'NONE',  ( -20.74285254778206067, 3.000000000000000000, 14.10762559394868099 ) ) ;
#2913 = VECTOR ( 'NONE', #11160, 1000.000000000000000 ) ;
#2914 = CARTESIAN_POINT ( 'NONE',  ( -5.999999999999991118, 0.000000000000000000, 27.00000000000000000 ) ) ;
#2915 = AXIS2_PLACEMENT_3D ( 'NONE', #6819, #8951, #11101 ) ;
#2916 = CIRCLE ( 'NONE', #10619, 12.08999999999737440 ) ;
#2917 = CARTESIAN_POINT ( 'NONE',  ( 2.601737331980797041, 9.000000000000000000, -6.888123234756056590 ) ) ;
#2918 = CARTESIAN_POINT ( 'NONE',  ( -13.28140389626389783, 3.000000000000000000, 13.39999999999999858 ) ) ;
#2919 = CARTESIAN_POINT ( 'NONE',  ( -12.68816982652953840, 0.000000000000000000, -2.830255545554093644 ) ) ;
#2920 = CONTEXT_DEPENDENT_SHAPE_REPRESENTATION ( #11001, #6454 ) ;
#2921 = DIRECTION ( 'NONE',  ( 0.000000000000000000, 0.000000000000000000, -1.000000000000000000 ) ) ;
#2922 = CARTESIAN_POINT ( 'NONE',  ( -14.82803603298502360, 3.000000000000000000, -2.264806262022826644 ) ) ;
#2923 = CARTESIAN_POINT ( 'NONE',  ( 52.12339130828321032, 3.000000000000000000, -4.353525159591052685 ) ) ;
#2924 = FACE_OUTER_BOUND ( 'NONE', #13436, .T. ) ;
#2925 = DIRECTION ( 'NONE',  ( 0.000000000000000000, 0.000000000000000000, 1.000000000000000000 ) ) ;
#2926 = ORIENTED_EDGE ( 'NONE', *, *, #11909, .F. ) ;
#2927 = EDGE_LOOP ( 'NONE', ( #3180, #5073, #2774, #3352 ) ) ;
#2928 = VECTOR ( 'NONE', #7246, 1000.000000000000000 ) ;
#2929 = ORIENTED_EDGE ( 'NONE', *, *, #11861, .T. ) ;
#2930 = B_SPLINE_CURVE_WITH_KNOTS ( 'NONE', 3,
 ( #7934, #2433, #4708, #8901 ),
 .UNSPECIFIED., .F., .F.,
 ( 4, 4 ),
 ( 0.1547128134717859205, 1.000000000000000000 ),
 .UNSPECIFIED. ) ;
#2931 = ORIENTED_EDGE ( 'NONE', *, *, #8943, .F. ) ;
#2932 = DIRECTION ( 'NONE',  ( -0.000000000000000000, -1.000000000000000000, -0.000000000000000000 ) ) ;
#2933 = SURFACE_SIDE_STYLE ('',( #10160 ) ) ;
#2934 = CIRCLE ( 'NONE', #4691, 3.400000000000001243 ) ;
#2935 = CARTESIAN_POINT ( 'NONE',  ( -14.87484884897975057, 3.000000000000000000, 1.958311002203303453 ) ) ;
#2936 = AXIS2_PLACEMENT_3D ( 'NONE', #7563, #5285, #203 ) ;
#2937 = DIRECTION ( 'NONE',  ( -0.000000000000000000, -1.000000000000000000, -0.000000000000000000 ) ) ;
#2938 = DIRECTION ( 'NONE',  ( 0.000000000000000000, 0.000000000000000000, -1.000000000000000000 ) ) ;
#2939 = EDGE_CURVE ( 'NONE', #6263, #1441, #9356, .T. ) ;
#2940 = DIRECTION ( 'NONE',  ( -0.000000000000000000, -1.000000000000000000, -0.000000000000000000 ) ) ;
#2941 = LINE ( 'NONE', #8039, #7994 ) ;
#2942 = ORIENTED_EDGE ( 'NONE', *, *, #7785, .T. ) ;
#2943 = CARTESIAN_POINT ( 'NONE',  ( 5.051606143860416509, 9.000000000000000000, 4.477027514692274224 ) ) ;
#2944 = VECTOR ( 'NONE', #11871, 1000.000000000000000 ) ;
#2945 = CARTESIAN_POINT ( 'NONE',  ( -5.452638258930639914, 3.000000000000000000, -13.97385902380748313 ) ) ;
#2946 = VECTOR ( 'NONE', #4621, 1000.000000000000000 ) ;
#2947 = EDGE_LOOP ( 'NONE', ( #11195, #11654, #6079, #11465 ) ) ;
#2948 = CYLINDRICAL_SURFACE ( 'NONE', #11212, 6.750000000000001776 ) ;
#2949 = DIRECTION ( 'NONE',  ( 0.3534274726160315794, 1.141457706935629186E-21, -0.9354619295301355164 ) ) ;
#2950 = EDGE_CURVE ( 'NONE', #500, #8456, #83, .T. ) ;
#2951 = CARTESIAN_POINT ( 'NONE',  ( 1.105736515254441388, 3.000000000000000000, -13.50994833511691695 ) ) ;
#2952 = LINE ( 'NONE', #4954, #9251 ) ;
#2953 = EDGE_CURVE ( 'NONE', #10793, #3691, #3271, .T. ) ;
#2955 = ADVANCED_FACE ( 'NONE', ( #5364 ), #9634, .T. ) ;
#2954 = AXIS2_PLACEMENT_3D ( 'NONE', #6047, #9344, #4039 ) ;
#2956 = PLANE ( 'NONE',  #12210 ) ;
#2957 = VECTOR ( 'NONE', #2879, 1000.000000000000000 ) ;
#2958 = CARTESIAN_POINT ( 'NONE',  ( 2.830255545554135832, 0.000000000000000000, -12.68816982652952596 ) ) ;
#2959 = CARTESIAN_POINT ( 'NONE',  ( -12.40340517008309185, 0.000000000000000000, -3.893011711613028947 ) ) ;
#2960 = CARTESIAN_POINT ( 'NONE',  ( 6.554160776451332993, 9.000000000000000000, -1.614148852004323675 ) ) ;
#2961 = EDGE_CURVE ( 'NONE', #1437, #4866, #10766, .T. ) ;
#2962 = ORIENTED_EDGE ( 'NONE', *, *, #955, .F. ) ;
#2963 = ORIENTED_EDGE ( 'NONE', *, *, #13274, .T. ) ;
#2964 = VERTEX_POINT ( 'NONE', #2193 ) ;
#2965 = CARTESIAN_POINT ( 'NONE',  ( -14.90895795148409420, 3.000000000000000000, 1.650143266773909101 ) ) ;
#2966 = ORIENTED_EDGE ( 'NONE', *, *, #6648, .T. ) ;
#2967 = CIRCLE ( 'NONE', #6264, 2.500000000000000000 ) ;
#2968 = AXIS2_PLACEMENT_3D ( 'NONE', #574, #7855, #1602 ) ;
#2969 = CARTESIAN_POINT ( 'NONE',  ( -8.922226997226788470, 3.000000000000000000, -8.158551673544387484 ) ) ;
#2970 = CARTESIAN_POINT ( 'NONE',  ( 53.04054522416362261, 3.000000000000000000, -3.611077387296437013 ) ) ;
#2971 = ADVANCED_FACE ( 'NONE', ( #8587 ), #1712, .T. ) ;
#2972 = CARTESIAN_POINT ( 'NONE',  ( 0.4639228963249704130, 0.000000000000000000, 8.487330295579726069 ) ) ;
#2973 = CYLINDRICAL_SURFACE ( 'NONE', #9759, 14.25000000000000178 ) ;
#2974 = CARTESIAN_POINT ( 'NONE',  ( 1.580708947611198623, 0.000000000000000000, -8.351727918397600092 ) ) ;
#2975 = CARTESIAN_POINT ( 'NONE',  ( 17.00000000000000711, 3.000000000000000000, 12.57924256039205524 ) ) ;
#2976 = VERTEX_POINT ( 'NONE', #3286 ) ;
#2977 = EDGE_CURVE ( 'NONE', #2583, #8871, #4167, .T. ) ;
#2978 = DIRECTION ( 'NONE',  ( -0.000000000000000000, -1.000000000000000000, 0.000000000000000000 ) ) ;
#2979 = CIRCLE ( 'NONE', #138, 8.499999999999998224 ) ;
#2980 = EDGE_CURVE ( 'NONE', #117, #5803, #1310, .T. ) ;
#2981 = ORIENTED_EDGE ( 'NONE', *, *, #2823, .T. ) ;
#2982 = ORIENTED_EDGE ( 'NONE', *, *, #13134, .T. ) ;
#2983 = LINE ( 'NONE', #1816, #7970 ) ;
#2985 = ORIENTED_EDGE ( 'NONE', *, *, #11508, .T. ) ;
#2984 = B_SPLINE_CURVE_WITH_KNOTS ( 'NONE', 3,
 ( #11290, #1858, #6059, #680 ),
 .UNSPECIFIED., .F., .F.,
 ( 4, 4 ),
 ( 0.000000000000000000, 0.8452273900860258760 ),
 .UNSPECIFIED. ) ;
#2986 = DIRECTION ( 'NONE',  ( 0.000000000000000000, 0.000000000000000000, 1.000000000000000000 ) ) ;
#2987 = STYLED_ITEM ( 'NONE', ( #3493 ), #12787 ) ;
#2988 = CARTESIAN_POINT ( 'NONE',  ( 10.25006213149504752, 3.000000000000000000, -9.299128225235653744 ) ) ;
#2989 = CARTESIAN_POINT ( 'NONE',  ( -20.74285254778206422, 0.000000000000000000, 14.10762559394868454 ) ) ;
#2990 = DIRECTION ( 'NONE',  ( 0.000000000000000000, 0.000000000000000000, 1.000000000000000000 ) ) ;
#2991 = LINE ( 'NONE', #11395, #5277 ) ;
#2992 = CARTESIAN_POINT ( 'NONE',  ( 4.164551629694410728, 0.000000000000000000, -6.072874324029720050 ) ) ;
#2993 = CARTESIAN_POINT ( 'NONE',  ( -8.883544964652065445, 3.000000000000000000, -12.08646469655229438 ) ) ;
#2994 = CARTESIAN_POINT ( 'NONE',  ( -11.80612203322752585, 3.000000000000000000, 2.604531154829235362 ) ) ;
#2995 = B_SPLINE_CURVE_WITH_KNOTS ( 'NONE', 2,
 ( #6104, #938, #3125 ),
 .UNSPECIFIED., .F., .F.,
 ( 3, 3 ),
 ( 0.000000000000000000, 1.000000000000000000 ),
 .UNSPECIFIED. ) ;
#2996 = ORIENTED_EDGE ( 'NONE', *, *, #7201, .F. ) ;
#2997 = CARTESIAN_POINT ( 'NONE',  ( -2.481593227817846525, 9.000000000000000000, -8.129679886173168057 ) ) ;
#2998 = VERTEX_POINT ( 'NONE', #12548 ) ;
#2999 = PRODUCT_DEFINITION_FORMATION_WITH_SPECIFIED_SOURCE ( 'ANY', '', #10857, .NOT_KNOWN. ) ;
#3000 = ORIENTED_EDGE ( 'NONE', *, *, #1698, .F. ) ;
#3001 = ORIENTED_EDGE ( 'NONE', *, *, #9490, .T. ) ;
#3002 = ORIENTED_EDGE ( 'NONE', *, *, #10108, .F. ) ;
#3003 = CARTESIAN_POINT ( 'NONE',  ( -1.557181465540221188, 0.000000000000000000, 14.16466328168015743 ) ) ;
#3004 = FACE_OUTER_BOUND ( 'NONE', #10795, .T. ) ;
#3005 = EDGE_CURVE ( 'NONE', #1142, #3822, #3941, .T. ) ;
#3006 = EDGE_CURVE ( 'NONE', #3264, #2583, #3068, .T. ) ;
#3007 = CARTESIAN_POINT ( 'NONE',  ( -12.08646469655240097, 3.000000000000000000, -8.883544964651921561 ) ) ;
#3008 = FACE_BOUND ( 'NONE', #9102, .T. ) ;
#3009 = DIRECTION ( 'NONE',  ( 0.000000000000000000, 0.000000000000000000, -1.000000000000000000 ) ) ;
#3010 = CARTESIAN_POINT ( 'NONE',  ( 6.506507307819716424, 3.000000000000000000, -10.18987059060247269 ) ) ;
#3011 = DIRECTION ( 'NONE',  ( 0.000000000000000000, 0.000000000000000000, 1.000000000000000000 ) ) ;
#3012 = ORIENTED_EDGE ( 'NONE', *, *, #8840, .T. ) ;
#3013 = DIRECTION ( 'NONE',  ( -0.000000000000000000, -1.000000000000000000, -0.000000000000000000 ) ) ;
#3014 = CYLINDRICAL_SURFACE ( 'NONE', #7545, 6.750000000000000888 ) ;
#3015 = ORIENTED_EDGE ( 'NONE', *, *, #12897, .F. ) ;
#3016 = CARTESIAN_POINT ( 'NONE',  ( 12.25836857253663581, 0.000000000000000000, 5.784789447945493990 ) ) ;
#3017 = DIRECTION ( 'NONE',  ( 0.000000000000000000, 0.000000000000000000, 1.000000000000000000 ) ) ;
#3018 = CARTESIAN_POINT ( 'NONE',  ( -14.08504230442587790, 3.000000000000000000, -2.161962830978695571 ) ) ;
#3019 = CARTESIAN_POINT ( 'NONE',  ( 2.428572470324196431, 0.000000000000000000, 13.33579367773357127 ) ) ;
#3020 = CARTESIAN_POINT ( 'NONE',  ( -10.33484986938308303, 0.000000000000000000, 8.771102293099071190 ) ) ;
#3021 = CARTESIAN_POINT ( 'NONE',  ( 13.50000000000000355, 3.000000000000000000, -5.550000000000001599 ) ) ;
#3022 = CARTESIAN_POINT ( 'NONE',  ( -12.16218796965919324, 3.000000000000000000, -4.056222772158363021 ) ) ;
#3023 = VERTEX_POINT ( 'NONE', #3161 ) ;
#3024 = ORIENTED_EDGE ( 'NONE', *, *, #13248, .T. ) ;
#3025 = CARTESIAN_POINT ( 'NONE',  ( -6.506507307819711095, 0.000000000000000000, 10.18987059060247624 ) ) ;
#3026 = EDGE_CURVE ( 'NONE', #7708, #13219, #4190, .T. ) ;
#3027 = ORIENTED_EDGE ( 'NONE', *, *, #11120, .T. ) ;
#3028 = PRODUCT_DEFINITION ( 'UNKNOWN', '', #1684, #1457 ) ;
#3029 = B_SPLINE_SURFACE_WITH_KNOTS ( 'NONE', 3, 1, ( 
 ( #10782, #586 ),
 ( #11761, #7937 ),
 ( #2779, #1350 ),
 ( #6986, #8644 ) ),
 .UNSPECIFIED., .F., .F., .F.,
 ( 4, 4 ),
 ( 2, 2 ),
 ( 0.000000000000000000, 0.8724294488011762327 ),
 ( 0.000000000000000000, 1.000000000000000000 ),
 .UNSPECIFIED. ) ;
#3030 = FACE_OUTER_BOUND ( 'NONE', #13111, .T. ) ;
#3031 = DIRECTION ( 'NONE',  ( -0.000000000000000000, -1.000000000000000000, -0.000000000000000000 ) ) ;
#3032 = DIRECTION ( 'NONE',  ( 0.000000000000000000, 0.000000000000000000, -1.000000000000000000 ) ) ;
#3033 = CARTESIAN_POINT ( 'NONE',  ( -3.542894779577211661, 0.000000000000000000, -12.51336118825813948 ) ) ;
#3034 = CARTESIAN_POINT ( 'NONE',  ( 1.127406311874972422, 9.000000000000000000, -7.862174656777307646 ) ) ;
#3035 = CARTESIAN_POINT ( 'NONE',  ( -5.999999999999991118, 0.000000000000000000, 27.00000000000000000 ) ) ;
#3036 = ORIENTED_EDGE ( 'NONE', *, *, #10962, .T. ) ;
#3037 = CARTESIAN_POINT ( 'NONE',  ( 31.00000000000000000, 3.000000000000000000, 0.000000000000000000 ) ) ;
#3038 = EDGE_LOOP ( 'NONE', ( #11382, #2337, #10364, #5538 ) ) ;
#3039 = ORIENTED_EDGE ( 'NONE', *, *, #5146, .T. ) ;
#3040 = CARTESIAN_POINT ( 'NONE',  ( 8.093005444143644311, 9.000000000000000000, -2.598704077239528232 ) ) ;
#3041 = EDGE_CURVE ( 'NONE', #2033, #12313, #8992, .T. ) ;
#3042 = ORIENTED_EDGE ( 'NONE', *, *, #13411, .T. ) ;
#3043 = LINE ( 'NONE', #2912, #3168 ) ;
#3044 = EDGE_CURVE ( 'NONE', #3304, #2066, #9831, .T. ) ;
#3045 = LINE ( 'NONE', #2152, #2756 ) ;
#3046 = EDGE_CURVE ( 'NONE', #597, #655, #820, .T. ) ;
#3047 = DIRECTION ( 'NONE',  ( 0.5366322685380732205, 0.000000000000000000, 0.8438162171727212613 ) ) ;
#3048 = CARTESIAN_POINT ( 'NONE',  ( 7.702138240596516638, 3.000000000000000000, -27.99999999999999289 ) ) ;
#3049 = CARTESIAN_POINT ( 'NONE',  ( 0.000000000000000000, 3.000000000000000000, 0.000000000000000000 ) ) ;
#3050 = DIRECTION ( 'NONE',  ( -0.000000000000000000, -1.000000000000000000, -0.000000000000000000 ) ) ;
#3051 = CARTESIAN_POINT ( 'NONE',  ( -7.077546079049271910, 3.000000000000000000, -10.67828022838850544 ) ) ;
#3052 = DIRECTION ( 'NONE',  ( -0.000000000000000000, 1.000000000000000000, -0.000000000000000000 ) ) ;
#3053 = ORIENTED_EDGE ( 'NONE', *, *, #3579, .T. ) ;
#3054 = DIRECTION ( 'NONE',  ( 0.000000000000000000, 0.000000000000000000, -1.000000000000000000 ) ) ;
#3055 = ORIENTED_EDGE ( 'NONE', *, *, #596, .T. ) ;
#3056 = AXIS2_PLACEMENT_3D ( 'NONE', #10125, #12284, #971 ) ;
#3057 = ORIENTED_EDGE ( 'NONE', *, *, #1569, .F. ) ;
#3058 = CIRCLE ( 'NONE', #8763, 0.9999999999999991118 ) ;
#3059 = ADVANCED_FACE ( 'NONE', ( #6601 ), #1505, .F. ) ;
#3060 = EDGE_LOOP ( 'NONE', ( #8091, #7329, #1726, #1387 ) ) ;
#3061 = EDGE_LOOP ( 'NONE', ( #9173, #356, #12170, #6925 ) ) ;
#3062 = DIRECTION ( 'NONE',  ( 0.000000000000000000, 0.000000000000000000, 1.000000000000000000 ) ) ;
#3063 = CARTESIAN_POINT ( 'NONE',  ( -8.795158114916672432, 0.000000000000000000, -9.573149624528774382 ) ) ;
#3064 = EDGE_CURVE ( 'NONE', #4996, #4061, #8364, .T. ) ;
#3065 = DIRECTION ( 'NONE',  ( 0.000000000000000000, 0.000000000000000000, 1.000000000000000000 ) ) ;
#3066 = CARTESIAN_POINT ( 'NONE',  ( -10.18979803820052155, 3.000000000000000000, 6.506620931068709091 ) ) ;
#3067 = DIRECTION ( 'NONE',  ( 0.000000000000000000, 1.000000000000000000, -0.000000000000000000 ) ) ;
#3068 = CIRCLE ( 'NONE', #12753, 3.400000000000001243 ) ;
#3069 = EDGE_LOOP ( 'NONE', ( #8602, #1980, #6687, #5840 ) ) ;
#3070 = EDGE_CURVE ( 'NONE', #2033, #8075, #470, .T. ) ;
#3071 = CARTESIAN_POINT ( 'NONE',  ( -5.250000000000000000, 3.000000000000000000, -27.94078293894052578 ) ) ;
#3072 = CARTESIAN_POINT ( 'NONE',  ( -3.542894779577211661, 0.000000000000000000, -12.51336118825813948 ) ) ;
#3073 = EDGE_LOOP ( 'NONE', ( #8720, #10119, #5212, #1076 ) ) ;
#3074 = CARTESIAN_POINT ( 'NONE',  ( -7.155006492985575228, 0.000000000000000000, -1.740452503570284915 ) ) ;
#3075 = CIRCLE ( 'NONE', #5088, 8.499999999999992895 ) ;
#3076 = AXIS2_PLACEMENT_3D ( 'NONE', #1054, #6146, #2990 ) ;
#3077 = CARTESIAN_POINT ( 'NONE',  ( -3.647599401157625376, 3.000000000000000000, -11.52662650599085836 ) ) ;
#3078 = DIRECTION ( 'NONE',  ( -0.8297244024006588115, 5.023789833012348328E-26, 0.5581732849759741821 ) ) ;
#3079 = DIRECTION ( 'NONE',  ( 0.000000000000000000, 0.000000000000000000, 1.000000000000000000 ) ) ;
#3080 = CARTESIAN_POINT ( 'NONE',  ( 0.000000000000000000, 0.000000000000000000, 0.000000000000000000 ) ) ;
#3081 = DIRECTION ( 'NONE',  ( 1.000000000000000000, 0.000000000000000000, 0.000000000000000000 ) ) ;
#3082 = AXIS2_PLACEMENT_3D ( 'NONE', #3360, #3227, #6536 ) ;
#3083 = DIRECTION ( 'NONE',  ( -1.000000000000000000, -0.000000000000000000, -1.927470528863118802E-16 ) ) ;
#3084 = CARTESIAN_POINT ( 'NONE',  ( -8.922226997226891498, 3.000000000000000000, -8.158551673544284455 ) ) ;
#3085 = CIRCLE ( 'NONE', #12981, 0.1000000000000001166 ) ;
#3086 = VERTEX_POINT ( 'NONE', #11986 ) ;
#3087 = VERTEX_POINT ( 'NONE', #5769 ) ;
#3088 = DIRECTION ( 'NONE',  ( -0.000000000000000000, -1.000000000000000000, -0.000000000000000000 ) ) ;
#3089 = VERTEX_POINT ( 'NONE', #12118 ) ;
#3090 = CARTESIAN_POINT ( 'NONE',  ( 0.000000000000000000, 0.000000000000000000, 0.000000000000000000 ) ) ;
#3091 = VECTOR ( 'NONE', #3849, 1000.000000000000114 ) ;
#3092 = CARTESIAN_POINT ( 'NONE',  ( -10.18987059060247624, 0.000000000000000000, -6.506507307819711095 ) ) ;
#3093 = CARTESIAN_POINT ( 'NONE',  ( -12.98835496148321944, 3.000000000000000000, -0.5501230721522551992 ) ) ;
#3094 = CIRCLE ( 'NONE', #1790, 1.500000000000000222 ) ;
#3095 = CARTESIAN_POINT ( 'NONE',  ( 3.469446951953614189E-15, 3.000000000000000000, -20.55000000000000071 ) ) ;
#3096 = CARTESIAN_POINT ( 'NONE',  ( 9.379342464487701037, 3.000000000000000000, -10.98198414889939301 ) ) ;
#3097 = CARTESIAN_POINT ( 'NONE',  ( -5.170206418547658167, 0.000000000000000000, -13.27898586450066887 ) ) ;
#3098 = ADVANCED_FACE ( 'NONE', ( #5491 ), #9699, .T. ) ;
#3099 = EDGE_LOOP ( 'NONE', ( #12485, #7712, #865, #8, #13124, #4158 ) ) ;
#3100 = CARTESIAN_POINT ( 'NONE',  ( -2.632142621505047408, 0.000000000000000000, -6.877144614729746586 ) ) ;
#3101 = EDGE_LOOP ( 'NONE', ( #12387, #11429 ) ) ;
#3102 = ORIENTED_EDGE ( 'NONE', *, *, #6600, .T. ) ;
#3103 = DIRECTION ( 'NONE',  ( -0.000000000000000000, -1.000000000000000000, -0.000000000000000000 ) ) ;
#3104 = AXIS2_PLACEMENT_3D ( 'NONE', #8100, #11272, #1845 ) ;
#3105 = ORIENTED_EDGE ( 'NONE', *, *, #4072, .F. ) ;
#3106 = DIRECTION ( 'NONE',  ( 0.000000000000000000, 0.000000000000000000, 1.000000000000000000 ) ) ;
#3107 = CARTESIAN_POINT ( 'NONE',  ( -21.21140389626389577, 3.000000000000000000, -14.83930531255815133 ) ) ;
#3108 = DIRECTION ( 'NONE',  ( -0.000000000000000000, -1.000000000000000000, -0.000000000000000000 ) ) ;
#3109 = DIRECTION ( 'NONE',  ( 0.000000000000000000, 1.000000000000000000, 0.000000000000000000 ) ) ;
#3110 = CARTESIAN_POINT ( 'NONE',  ( -5.571313494980132397, 0.000000000000000000, 10.72979803820132005 ) ) ;
#3111 = DIRECTION ( 'NONE',  ( -0.000000000000000000, -1.000000000000000000, -0.000000000000000000 ) ) ;
#3112 = VECTOR ( 'NONE', #12814, 1000.000000000000000 ) ;
#3113 = EDGE_CURVE ( 'NONE', #6069, #10836, #6586, .T. ) ;
#3114 = CARTESIAN_POINT ( 'NONE',  ( -8.430890348300632553, 3.000000000000000000, -11.48836750521723538 ) ) ;
#3115 = PLANE ( 'NONE',  #10237 ) ;
#3116 = VERTEX_POINT ( 'NONE', #2666 ) ;
#3117 = CARTESIAN_POINT ( 'NONE',  ( -10.97318381393799136, 3.000000000000000000, -6.970598036433411693 ) ) ;
#3118 = ORIENTED_EDGE ( 'NONE', *, *, #4381, .T. ) ;
#3119 = ORIENTED_EDGE ( 'NONE', *, *, #1269, .T. ) ;
#3120 = ADVANCED_FACE ( 'NONE', ( #3564, #11005, #6676 ), #12050, .F. ) ;
#3121 = ORIENTED_EDGE ( 'NONE', *, *, #5398, .F. ) ;
#3122 = AXIS2_PLACEMENT_3D ( 'NONE', #11280, #12531, #7157 ) ;
#3123 = AXIS2_PLACEMENT_3D ( 'NONE', #9612, #7674, #383 ) ;
#3124 = VERTEX_POINT ( 'NONE', #1444 ) ;
#3125 = CARTESIAN_POINT ( 'NONE',  ( -12.08646469655240097, 0.000000000000000000, -8.883544964651921561 ) ) ;
#3126 = CARTESIAN_POINT ( 'NONE',  ( 26.30958424017656938, 0.000000000000000000, -4.500000000000000888 ) ) ;
#3127 = EDGE_CURVE ( 'NONE', #2851, #3598, #12546, .T. ) ;
#3128 = CARTESIAN_POINT ( 'NONE',  ( 8.158651161643900807, 3.000000000000000000, 8.922136023539609440 ) ) ;
#3129 = CARTESIAN_POINT ( 'NONE',  ( 0.000000000000000000, 3.000000000000000000, -1.500000000000000222 ) ) ;
#3130 = VECTOR ( 'NONE', #2699, 1000.000000000000000 ) ;
#3131 = VECTOR ( 'NONE', #5384, 1000.000000000000000 ) ;
#3132 = AXIS2_PLACEMENT_3D ( 'NONE', #8812, #10966, #10068 ) ;
#3133 = ORIENTED_EDGE ( 'NONE', *, *, #11069, .T. ) ;
#3134 = VERTEX_POINT ( 'NONE', #275 ) ;
#3135 = ADVANCED_FACE ( 'NONE', ( #7771 ), #5634, .T. ) ;
#3136 = CARTESIAN_POINT ( 'NONE',  ( -11.14709020439930676, 3.000000000000000000, -7.712570079660886257 ) ) ;
#3137 = FACE_OUTER_BOUND ( 'NONE', #11415, .T. ) ;
#3138 = EDGE_LOOP ( 'NONE', ( #10170, #206, #8007, #10135 ) ) ;
#3139 = CARTESIAN_POINT ( 'NONE',  ( 5.250000000000000000, 3.000000000000000000, -27.94078293894052578 ) ) ;
#3140 = PRODUCT_DEFINITION_SHAPE ( 'NONE', 'NONE',  #3028 ) ;
#3141 = TOROIDAL_SURFACE ( 'NONE', #3573, 3.100000000000000533, 0.1000000000000000056 ) ;
#3142 = AXIS2_PLACEMENT_3D ( 'NONE', #11090, #5854, #1514 ) ;
#3143 = CARTESIAN_POINT ( 'NONE',  ( 20.00000000000000711, 3.000000000000000000, 12.57924256039204280 ) ) ;
#3144 = SHAPE_DEFINITION_REPRESENTATION ( #11056, #2323 ) ;
#3145 = EDGE_CURVE ( 'NONE', #205, #4996, #2853, .T. ) ;
#3146 = CARTESIAN_POINT ( 'NONE',  ( 8.180229652970799847, 0.000000000000000000, -11.90209577080762848 ) ) ;
#3147 = CARTESIAN_POINT ( 'NONE',  ( 12.90250726680438476, 3.000000000000000000, 4.728042766759046778 ) ) ;
#3148 = EDGE_CURVE ( 'NONE', #11517, #2610, #13081, .T. ) ;
#3149 = FACE_BOUND ( 'NONE', #3474, .T. ) ;
#3150 = B_SPLINE_CURVE_WITH_KNOTS ( 'NONE', 3,
 ( #12535, #3074, #7288, #6888 ),
 .UNSPECIFIED., .F., .F.,
 ( 4, 4 ),
 ( 0.000000000000000000, 0.8724294488011763438 ),
 .UNSPECIFIED. ) ;
#3151 = DIRECTION ( 'NONE',  ( -0.000000000000000000, -1.000000000000000000, -0.000000000000000000 ) ) ;
#3152 = AXIS2_PLACEMENT_3D ( 'NONE', #9011, #5216, #11229 ) ;
#3153 = CARTESIAN_POINT ( 'NONE',  ( -8.883544964652065445, 0.000000000000000000, -12.08646469655229438 ) ) ;
#3154 = CIRCLE ( 'NONE', #3584, 0.1000000000000000472 ) ;
#3155 = AXIS2_PLACEMENT_3D ( 'NONE', #7761, #9960, #9886 ) ;
#3156 = ORIENTED_EDGE ( 'NONE', *, *, #7047, .T. ) ;
#3157 = ORIENTED_EDGE ( 'NONE', *, *, #10543, .T. ) ;
#3158 = EDGE_LOOP ( 'NONE', ( #7301, #8563, #4698, #6630 ) ) ;
#3159 = CARTESIAN_POINT ( 'NONE',  ( 10.14701493152832512, 0.000000000000000000, -29.73855628788322747 ) ) ;
#3160 = ORIENTED_EDGE ( 'NONE', *, *, #1366, .F. ) ;
#3161 = CARTESIAN_POINT ( 'NONE',  ( 5.250000000000000000, 3.000000000000000000, -26.44078293894052578 ) ) ;
#3162 = AXIS2_PLACEMENT_3D ( 'NONE', #7275, #5959, #2038 ) ;
#3163 = CIRCLE ( 'NONE', #6904, 14.25000000000000178 ) ;
#3164 = CARTESIAN_POINT ( 'NONE',  ( -12.14623037080100865, 0.000000000000000000, 4.072642252455982437 ) ) ;
#3165 = EDGE_CURVE ( 'NONE', #8551, #8134, #3635, .T. ) ;
#3166 = CARTESIAN_POINT ( 'NONE',  ( 5.571313494980134173, 3.000000000000000000, -10.72979803820132005 ) ) ;
#3167 = EDGE_CURVE ( 'NONE', #868, #1536, #5731, .T. ) ;
#3168 = VECTOR ( 'NONE', #5041, 1000.000000000000000 ) ;
#3169 = CARTESIAN_POINT ( 'NONE',  ( 0.6724118135762067183, 0.000000000000000000, -13.82336506795094344 ) ) ;
#3170 = LINE ( 'NONE', #4272, #3112 ) ;
#3171 = CARTESIAN_POINT ( 'NONE',  ( -12.25836857253663759, 3.000000000000000000, -5.784789447945487773 ) ) ;
#3172 = ORIENTED_EDGE ( 'NONE', *, *, #11194, .T. ) ;
#3173 = PLANE ( 'NONE',  #6883 ) ;
#3174 = EDGE_LOOP ( 'NONE', ( #6209, #10903, #3648, #5215 ) ) ;
#3175 = ORIENTED_EDGE ( 'NONE', *, *, #11211, .T. ) ;
#3176 = VECTOR ( 'NONE', #8703, 1000.000000000000000 ) ;
#3177 = ORIENTED_EDGE ( 'NONE', *, *, #9550, .T. ) ;
#3178 = CIRCLE ( 'NONE', #6255, 2.999999999999999112 ) ;
#3179 = CARTESIAN_POINT ( 'NONE',  ( 48.80418793193314997, 3.000000000000000000, -4.004112872419501201 ) ) ;
#3180 = ORIENTED_EDGE ( 'NONE', *, *, #8860, .F. ) ;
#3181 = B_SPLINE_CURVE_WITH_KNOTS ( 'NONE', 2,
 ( #11637, #5362, #5167 ),
 .UNSPECIFIED., .F., .F.,
 ( 3, 3 ),
 ( 0.000000000000000000, 1.000000000000000000 ),
 .UNSPECIFIED. ) ;
#3182 = EDGE_CURVE ( 'NONE', #10584, #479, #5564, .T. ) ;
#3183 = CARTESIAN_POINT ( 'NONE',  ( -13.33788847341978645, 0.000000000000000000, -2.414978278956336322 ) ) ;
#3184 = CARTESIAN_POINT ( 'NONE',  ( 2.719999999999997087, 2.000000000000000000, -6.000000000000000000 ) ) ;
#3185 = DIRECTION ( 'NONE',  ( 0.000000000000000000, 1.000000000000000000, 0.000000000000000000 ) ) ;
#3186 = DIRECTION ( 'NONE',  ( 1.224646799147353207E-16, 0.000000000000000000, -1.000000000000000000 ) ) ;
#3187 = CARTESIAN_POINT ( 'NONE',  ( -2.655466033450426533, 0.000000000000000000, -7.485541762018160128 ) ) ;
#3188 = MECHANICAL_DESIGN_GEOMETRIC_PRESENTATION_REPRESENTATION (  '', ( #2527 ), #4076 ) ;
#3189 = CARTESIAN_POINT ( 'NONE',  ( -5.976238463952679325, 0.000000000000000000, -3.138004751744733589 ) ) ;
#3190 = CIRCLE ( 'NONE', #131, 12.08999999999737440 ) ;
#3191 = PLANE ( 'NONE',  #6195 ) ;
#3192 = DIRECTION ( 'NONE',  ( -0.000000000000000000, -1.000000000000000000, -0.000000000000000000 ) ) ;
#3193 = ORIENTED_EDGE ( 'NONE', *, *, #13411, .F. ) ;
#3194 = CARTESIAN_POINT ( 'NONE',  ( -8.922226997226788470, 0.000000000000000000, -8.158551673544387484 ) ) ;
#3195 = VERTEX_POINT ( 'NONE', #11213 ) ;
#3196 = VERTEX_POINT ( 'NONE', #5013 ) ;
#3197 = ORIENTED_EDGE ( 'NONE', *, *, #3974, .F. ) ;
#3198 = AXIS2_PLACEMENT_3D ( 'NONE', #11150, #1719, #11006 ) ;
#3199 = VECTOR ( 'NONE', #11440, 1000.000000000000000 ) ;
#3200 = EDGE_CURVE ( 'NONE', #12067, #7218, #11004, .T. ) ;
#3201 = VERTEX_POINT ( 'NONE', #12331 ) ;
#3202 = DIRECTION ( 'NONE',  ( 0.000000000000000000, -0.000000000000000000, 1.000000000000000000 ) ) ;
#3203 = DIRECTION ( 'NONE',  ( 0.000000000000000000, 0.000000000000000000, -1.000000000000000000 ) ) ;
#3204 = DIRECTION ( 'NONE',  ( 1.000000000000000000, 0.000000000000000000, -0.000000000000000000 ) ) ;
#3205 = DIRECTION ( 'NONE',  ( 0.000000000000000000, 0.000000000000000000, 1.000000000000000000 ) ) ;
#3206 = CARTESIAN_POINT ( 'NONE',  ( 17.00000000000000355, 3.000000000000000000, -14.92471123914605435 ) ) ;
#3207 = AXIS2_PLACEMENT_3D ( 'NONE', #11214, #5014, #5976 ) ;
#3208 = DIRECTION ( 'NONE',  ( 0.000000000000000000, 1.000000000000000000, 0.000000000000000000 ) ) ;
#3209 = ORIENTED_EDGE ( 'NONE', *, *, #9198, .T. ) ;
#3210 = VERTEX_POINT ( 'NONE', #4047 ) ;
#3211 = DIRECTION ( 'NONE',  ( 0.000000000000000000, 0.000000000000000000, 1.000000000000000000 ) ) ;
#3212 = ADVANCED_FACE ( 'NONE', ( #4949 ), #5907, .T. ) ;
#3213 = ORIENTED_EDGE ( 'NONE', *, *, #1453, .F. ) ;
#3214 = CARTESIAN_POINT ( 'NONE',  ( 2.458659560121116527, 9.000000000000000000, -8.136645080586040635 ) ) ;
#3215 = CARTESIAN_POINT ( 'NONE',  ( -4.072642252455976219, 3.000000000000000000, -12.14623037080101398 ) ) ;
#3216 = EDGE_CURVE ( 'NONE', #6730, #4765, #2305, .T. ) ;
#3217 = EDGE_CURVE ( 'NONE', #5437, #3986, #13288, .T. ) ;
#3218 = CARTESIAN_POINT ( 'NONE',  ( -5.452638258930639914, 0.000000000000000000, -13.97385902380748313 ) ) ;
#3219 = CARTESIAN_POINT ( 'NONE',  ( -8.222660081691577361, 3.000000000000000000, -5.549999999999999822 ) ) ;
#3220 = DIRECTION ( 'NONE',  ( 0.000000000000000000, 0.000000000000000000, 1.000000000000000000 ) ) ;
#3221 = CARTESIAN_POINT ( 'NONE',  ( 3.850308450823737516, 9.000000000000000000, 5.544152309732777617 ) ) ;
#3222 = ORIENTED_EDGE ( 'NONE', *, *, #795, .F. ) ;
#3223 = ORIENTED_EDGE ( 'NONE', *, *, #2279, .T. ) ;
#3224 = VERTEX_POINT ( 'NONE', #7973 ) ;
#3225 = DIRECTION ( 'NONE',  ( 0.000000000000000000, 1.000000000000000000, 0.000000000000000000 ) ) ;
#3226 = ORIENTED_EDGE ( 'NONE', *, *, #11688, .F. ) ;
#3227 = DIRECTION ( 'NONE',  ( 0.000000000000000000, -1.000000000000000000, 0.000000000000000000 ) ) ;
#3228 = B_SPLINE_SURFACE_WITH_KNOTS ( 'NONE', 3, 1, ( 
 ( #3938, #13251 ),
 ( #12299, #2841 ),
 ( #12372, #7052 ),
 ( #8010, #13530 ) ),
 .UNSPECIFIED., .F., .F., .F.,
 ( 4, 4 ),
 ( 2, 2 ),
 ( 0.000000000000000000, 0.8452273900860258760 ),
 ( 0.000000000000000000, 1.000000000000000000 ),
 .UNSPECIFIED. ) ;
#3229 = CARTESIAN_POINT ( 'NONE',  ( -13.27898586450066709, 3.000000000000000000, 5.170206418547661720 ) ) ;
#3230 = CARTESIAN_POINT ( 'NONE',  ( 30.65246752842885058, 0.000000000000000000, -7.988606140548566437 ) ) ;
#3231 = CARTESIAN_POINT ( 'NONE',  ( -11.13895890373326836, 3.000000000000000000, 7.723663868796768028 ) ) ;
#3232 = CARTESIAN_POINT ( 'NONE',  ( -1.650143266773857142, 3.000000000000000000, -14.90895795148409952 ) ) ;
#3233 = DIRECTION ( 'NONE',  ( 0.000000000000000000, 0.000000000000000000, 1.000000000000000000 ) ) ;
#3234 = CARTESIAN_POINT ( 'NONE',  ( -10.72979803820132183, 3.000000000000000000, -5.571313494980132397 ) ) ;
#3235 = B_SPLINE_CURVE_WITH_KNOTS ( 'NONE', 3,
 ( #5395, #2499, #3252, #4425 ),
 .UNSPECIFIED., .F., .F.,
 ( 4, 4 ),
 ( 0.1276832474596238665, 1.000000000000000000 ),
 .UNSPECIFIED. ) ;
#3236 = ORIENTED_EDGE ( 'NONE', *, *, #12818, .F. ) ;
#3237 = CARTESIAN_POINT ( 'NONE',  ( 6.749972395921142621, 9.000000000000000000, -0.01930425607464712062 ) ) ;
#3238 = VERTEX_POINT ( 'NONE', #2875 ) ;
#3239 = ORIENTED_EDGE ( 'NONE', *, *, #1342, .T. ) ;
#3240 = B_SPLINE_CURVE_WITH_KNOTS ( 'NONE', 3,
 ( #13495, #2809, #4049, #11151 ),
 .UNSPECIFIED., .F., .F.,
 ( 4, 4 ),
 ( 0.1547128134717859205, 1.000000000000000000 ),
 .UNSPECIFIED. ) ;
#3241 = ORIENTED_EDGE ( 'NONE', *, *, #7675, .T. ) ;
#3242 = LINE ( 'NONE', #1950, #11944 ) ;
#3243 = ORIENTED_EDGE ( 'NONE', *, *, #9776, .T. ) ;
#3244 = DIRECTION ( 'NONE',  ( -0.000000000000000000, -1.000000000000000000, -0.000000000000000000 ) ) ;
#3245 = CARTESIAN_POINT ( 'NONE',  ( -12.40340517008309185, 3.000000000000000000, -3.893011711613028947 ) ) ;
#3246 = DIRECTION ( 'NONE',  ( 0.000000000000000000, 1.000000000000000000, 0.000000000000000000 ) ) ;
#3247 = DIRECTION ( 'NONE',  ( -0.000000000000000000, -1.000000000000000000, 0.000000000000000000 ) ) ;
#3248 = FACE_BOUND ( 'NONE', #6666, .T. ) ;
#3249 = CYLINDRICAL_SURFACE ( 'NONE', #8386, 3.000000000000000444 ) ;
#3250 = CARTESIAN_POINT ( 'NONE',  ( 5.517918333394296049, -1.694065894508600678E-18, 4.875228826198821253 ) ) ;
#3251 = ORIENTED_EDGE ( 'NONE', *, *, #872, .T. ) ;
#3252 = CARTESIAN_POINT ( 'NONE',  ( 2.620242232815953809, 9.000000000000000000, 6.881105251569436199 ) ) ;
#3253 = EDGE_LOOP ( 'NONE', ( #8598, #4261, #2872, #4102 ) ) ;
#3254 = VERTEX_POINT ( 'NONE', #1782 ) ;
#3255 = ORIENTED_EDGE ( 'NONE', *, *, #10238, .F. ) ;
#3256 = LINE ( 'NONE', #4433, #13060 ) ;
#3257 = CYLINDRICAL_SURFACE ( 'NONE', #12221, 14.25000000000000355 ) ;
#3258 = DIRECTION ( 'NONE',  ( -1.000000000000000000, 3.469446951953610639E-15, 2.602085213965210149E-16 ) ) ;
#3259 = CARTESIAN_POINT ( 'NONE',  ( 11.90284147956858085, 3.000000000000000000, -9.133371500908429752 ) ) ;
#3260 = CARTESIAN_POINT ( 'NONE',  ( 10.86210944460165528, 0.000000000000000000, 29.48017534571043541 ) ) ;
#3261 = CARTESIAN_POINT ( 'NONE',  ( 0.000000000000000000, 0.000000000000000000, 0.000000000000000000 ) ) ;
#3262 = ORIENTED_EDGE ( 'NONE', *, *, #4976, .T. ) ;
#3263 = EDGE_CURVE ( 'NONE', #9464, #1815, #12097, .T. ) ;
#3264 = VERTEX_POINT ( 'NONE', #7084 ) ;
#3265 = DIRECTION ( 'NONE',  ( 0.000000000000000000, 1.000000000000000000, 0.000000000000000000 ) ) ;
#3266 = ORIENTED_EDGE ( 'NONE', *, *, #4811, .T. ) ;
#3267 = CARTESIAN_POINT ( 'NONE',  ( -12.56843238770841786, 0.000000000000000000, 3.367671042046304741 ) ) ;
#3268 = CYLINDRICAL_SURFACE ( 'NONE', #1985, 1.500000000000000222 ) ;
#3269 = PLANE ( 'NONE',  #2214 ) ;
#3270 = CARTESIAN_POINT ( 'NONE',  ( 12.48034623170854474, 0.000000000000000000, 4.337627373772809491 ) ) ;
#3271 = CIRCLE ( 'NONE', #5270, 14.25000000000000000 ) ;
#3272 = CARTESIAN_POINT ( 'NONE',  ( -13.73660796332618261, 3.000000000000000000, -6.025412986832017204 ) ) ;
#3273 = DIRECTION ( 'NONE',  ( 0.000000000000000000, 1.000000000000000000, -0.000000000000000000 ) ) ;
#3274 = EDGE_CURVE ( 'NONE', #12645, #3761, #7687, .T. ) ;
#3275 = B_SPLINE_CURVE_WITH_KNOTS ( 'NONE', 3,
 ( #13362, #11216, #12197, #3770 ),
 .UNSPECIFIED., .F., .F.,
 ( 4, 4 ),
 ( 0.000000000000000000, 0.5855695330273008592 ),
 .UNSPECIFIED. ) ;
#3276 = CARTESIAN_POINT ( 'NONE',  ( 4.227250083625740729, 0.000000000000000000, -13.17831234185050526 ) ) ;
#3277 = VERTEX_POINT ( 'NONE', #10042 ) ;
#3278 = ORIENTED_EDGE ( 'NONE', *, *, #6955, .F. ) ;
#3279 = ADVANCED_FACE ( 'NONE', ( #821 ), #6990, .F. ) ;
#3280 = ORIENTED_EDGE ( 'NONE', *, *, #4776, .T. ) ;
#3281 = CARTESIAN_POINT ( 'NONE',  ( -2.604531154829235362, 3.000000000000000000, -11.80612203322752585 ) ) ;
#3282 = EDGE_CURVE ( 'NONE', #7408, #7832, #9449, .T. ) ;
#3283 = AXIS2_PLACEMENT_3D ( 'NONE', #5893, #1917, #9267 ) ;
#3284 = AXIS2_PLACEMENT_3D ( 'NONE', #12904, #1120, #3448 ) ;
#3285 = ORIENTED_EDGE ( 'NONE', *, *, #5922, .F. ) ;
#3286 = CARTESIAN_POINT ( 'NONE',  ( 47.14458624375820506, 3.000000000000000000, -3.829406728833672613 ) ) ;
#3287 = FACE_OUTER_BOUND ( 'NONE', #10688, .T. ) ;
#3288 = B_SPLINE_CURVE_WITH_KNOTS ( 'NONE', 3,
 ( #10356, #4216, #927, #8485 ),
 .UNSPECIFIED., .F., .F.,
 ( 4, 4 ),
 ( 0.000000000000000000, 0.8452273900860258760 ),
 .UNSPECIFIED. ) ;
#3289 = DIRECTION ( 'NONE',  ( 0.000000000000000000, 1.000000000000000000, 0.000000000000000000 ) ) ;
#3290 = CARTESIAN_POINT ( 'NONE',  ( -6.558450276537426404, 9.000000000000000000, -1.596630818375420757 ) ) ;
#3291 = CIRCLE ( 'NONE', #11000, 1.500000000000003997 ) ;
#3292 = EDGE_CURVE ( 'NONE', #288, #7860, #3501, .T. ) ;
#3293 = CARTESIAN_POINT ( 'NONE',  ( 41.67875868938293138, 0.000000000000000000, -6.066649533482935119 ) ) ;
#3294 = AXIS2_PLACEMENT_3D ( 'NONE', #9701, #10681, #10539 ) ;
#3295 = CARTESIAN_POINT ( 'NONE',  ( 8.795158114916441505, 0.000000000000000000, -9.573149624528689117 ) ) ;
#3296 = EDGE_LOOP ( 'NONE', ( #6577, #5303, #675, #4112 ) ) ;
#3297 = CARTESIAN_POINT ( 'NONE',  ( 3.818534268238711782, 9.000000000000000000, -5.566084444408534004 ) ) ;
#3298 = ORIENTED_EDGE ( 'NONE', *, *, #4056, .T. ) ;
#3299 = ADVANCED_FACE ( 'NONE', ( #8173 ), #2948, .T. ) ;
#3300 = ORIENTED_EDGE ( 'NONE', *, *, #12348, .F. ) ;
#3301 = ORIENTED_EDGE ( 'NONE', *, *, #7101, .F. ) ;
#3302 = DIRECTION ( 'NONE',  ( 0.000000000000000000, 1.000000000000000000, -0.000000000000000000 ) ) ;
#3303 = EDGE_CURVE ( 'NONE', #5027, #3357, #5081, .T. ) ;
#3304 = VERTEX_POINT ( 'NONE', #3766 ) ;
#3305 = AXIS2_PLACEMENT_3D ( 'NONE', #13148, #2748, #824 ) ;
#3306 = VECTOR ( 'NONE', #2389, 1000.000000000000000 ) ;
#3307 = CARTESIAN_POINT ( 'NONE',  ( 9.379342464487701037, 3.000000000000000000, -10.98198414889939301 ) ) ;
#3308 = CARTESIAN_POINT ( 'NONE',  ( 2.604531154829233586, 3.000000000000000000, 11.80612203322752585 ) ) ;
#3310 = CARTESIAN_POINT ( 'NONE',  ( -11.48836750521728689, 3.000000000000000000, -8.430890348300561499 ) ) ;
#3309 = B_SPLINE_CURVE_WITH_KNOTS ( 'NONE', 3,
 ( #6356, #8287, #3250, #2096 ),
 .UNSPECIFIED., .F., .F.,
 ( 4, 4 ),
 ( 0.1276832474596250877, 1.000000000000000000 ),
 .UNSPECIFIED. ) ;
#3311 = CARTESIAN_POINT ( 'NONE',  ( 10.97318381393774089, 3.000000000000000000, -6.970598036433387712 ) ) ;
#3312 = DIRECTION ( 'NONE',  ( 0.000000000000000000, 0.000000000000000000, 1.000000000000000000 ) ) ;
#3313 = FACE_OUTER_BOUND ( 'NONE', #3523, .T. ) ;
#3314 = EDGE_CURVE ( 'NONE', #13127, #7310, #993, .T. ) ;
#3315 = DIRECTION ( 'NONE',  ( -0.000000000000000000, -1.000000000000000000, -0.000000000000000000 ) ) ;
#3316 = ADVANCED_FACE ( 'NONE', ( #8246 ), #11079, .F. ) ;
#3317 = DIRECTION ( 'NONE',  ( 0.000000000000000000, 1.000000000000000000, -0.000000000000000000 ) ) ;
#3318 = VERTEX_POINT ( 'NONE', #4115 ) ;
#3319 = CARTESIAN_POINT ( 'NONE',  ( 5.250000000000000000, 3.000000000000000000, -29.44078293894052933 ) ) ;
#3320 = AXIS2_PLACEMENT_3D ( 'NONE', #7808, #13120, #1481 ) ;
#3321 = EDGE_LOOP ( 'NONE', ( #1646, #2276, #12954, #8028 ) ) ;
#3322 = B_SPLINE_CURVE_WITH_KNOTS ( 'NONE', 3,
 ( #9469, #126, #10371, #12528 ),
 .UNSPECIFIED., .F., .F.,
 ( 4, 4 ),
 ( 0.1276832474596231171, 1.000000000000000000 ),
 .UNSPECIFIED. ) ;
#3323 = ORIENTED_EDGE ( 'NONE', *, *, #8036, .F. ) ;
#3324 = VERTEX_POINT ( 'NONE', #6456 ) ;
#3325 = CARTESIAN_POINT ( 'NONE',  ( 10.18987059060247269, 0.000000000000000000, 6.506507307819714647 ) ) ;
#3326 = CARTESIAN_POINT ( 'NONE',  ( 2.623034112301249721, -1.694065894508600678E-18, -7.496701717520498853 ) ) ;
#3327 = VECTOR ( 'NONE', #12359, 1000.000000000000000 ) ;
#3328 = CARTESIAN_POINT ( 'NONE',  ( 7.363612555047485131, 9.000000000000000000, -0.02242701489043354146 ) ) ;
#3329 = B_SPLINE_SURFACE_WITH_KNOTS ( 'NONE', 3, 1, ( 
 ( #13594, #3110 ),
 ( #8283, #7325 ),
 ( #11528, #1898 ),
 ( #10351, #5047 ) ),
 .UNSPECIFIED., .F., .F., .F.,
 ( 4, 4 ),
 ( 2, 2 ),
 ( 0.1547128134717859205, 1.000000000000000000 ),
 ( 0.000000000000000000, 1.000000000000000000 ),
 .UNSPECIFIED. ) ;
#3330 = CARTESIAN_POINT ( 'NONE',  ( -8.222660081691577361, 3.000000000000000000, -8.549999999999998934 ) ) ;
#3331 = CARTESIAN_POINT ( 'NONE',  ( -11.70905276178463872, 0.000000000000000000, -9.375397774054366806 ) ) ;
#3332 = DIRECTION ( 'NONE',  ( 0.000000000000000000, 1.000000000000000000, 0.000000000000000000 ) ) ;
#3333 = ORIENTED_EDGE ( 'NONE', *, *, #13043, .T. ) ;
#3334 = ORIENTED_EDGE ( 'NONE', *, *, #3714, .T. ) ;
#3335 = EDGE_CURVE ( 'NONE', #12461, #4201, #6313, .T. ) ;
#3336 = CARTESIAN_POINT ( 'NONE',  ( 10.34346111134700585, 3.000000000000000000, 8.760376775873716326 ) ) ;
#3337 = B_SPLINE_SURFACE_WITH_KNOTS ( 'NONE', 3, 1, ( 
 ( #11118, #7053 ),
 ( #12158, #10974 ),
 ( #6770, #11253 ),
 ( #1687, #5879 ) ),
 .UNSPECIFIED., .F., .F., .F.,
 ( 4, 4 ),
 ( 2, 2 ),
 ( 0.000000000000000000, 0.8452273900860258760 ),
 ( 0.000000000000000000, 1.000000000000000000 ),
 .UNSPECIFIED. ) ;
#3338 = ORIENTED_EDGE ( 'NONE', *, *, #7784, .T. ) ;
#3339 = CARTESIAN_POINT ( 'NONE',  ( -8.922136023539609440, 0.000000000000000000, 8.158651161643900807 ) ) ;
#3340 = B_SPLINE_CURVE_WITH_KNOTS ( 'NONE', 3,
 ( #6905, #1889, #7191, #4980 ),
 .UNSPECIFIED., .F., .F.,
 ( 4, 4 ),
 ( 0.1276832474596244493, 1.000000000000000000 ),
 .UNSPECIFIED. ) ;
#3341 = EDGE_CURVE ( 'NONE', #7249, #2521, #6, .T. ) ;
#3342 = FACE_OUTER_BOUND ( 'NONE', #5858, .T. ) ;
#3343 = CIRCLE ( 'NONE', #1152, 8.499999999999998224 ) ;
#3344 = CIRCLE ( 'NONE', #943, 3.000000000000000888 ) ;
#3345 = AXIS2_PLACEMENT_3D ( 'NONE', #11461, #2030, #2161 ) ;
#3346 = DIRECTION ( 'NONE',  ( -1.000000000000000000, 0.000000000000000000, 0.000000000000000000 ) ) ;
#3347 = DIRECTION ( 'NONE',  ( -0.000000000000000000, -1.000000000000000000, -0.000000000000000000 ) ) ;
#3348 = DIRECTION ( 'NONE',  ( -0.6923076923076927347, 0.000000000000000000, 0.7216024245882196597 ) ) ;
#3349 = DIRECTION ( 'NONE',  ( 0.000000000000000000, 1.000000000000000000, -0.000000000000000000 ) ) ;
#3350 = CARTESIAN_POINT ( 'NONE',  ( 3.893011711613070691, 3.000000000000000000, -12.40340517008307231 ) ) ;
#3351 = ORIENTED_EDGE ( 'NONE', *, *, #5080, .T. ) ;
#3352 = ORIENTED_EDGE ( 'NONE', *, *, #8204, .F. ) ;
#3353 = AXIS2_PLACEMENT_3D ( 'NONE', #8518, #11773, #12941 ) ;
#3354 = ORIENTED_EDGE ( 'NONE', *, *, #4091, .F. ) ;
#3355 = CARTESIAN_POINT ( 'NONE',  ( 0.000000000000000000, 2.900000000000000355, 0.000000000000000000 ) ) ;
#3356 = AXIS2_PLACEMENT_3D ( 'NONE', #12930, #7625, #9752 ) ;
#3357 = VERTEX_POINT ( 'NONE', #5351 ) ;
#3358 = EDGE_CURVE ( 'NONE', #11145, #10549, #5045, .T. ) ;
#3359 = ADVANCED_FACE ( 'NONE', ( #5279 ), #8444, .F. ) ;
#3360 = CARTESIAN_POINT ( 'NONE',  ( -7.798201703419567643, 0.000000000000000000, -27.99999999999999289 ) ) ;
#3361 = SURFACE_SIDE_STYLE ('',( #1506 ) ) ;
#3362 = CARTESIAN_POINT ( 'NONE',  ( 0.000000000000000000, 3.000000000000000000, 0.000000000000000000 ) ) ;
#3363 = DIRECTION ( 'NONE',  ( 0.000000000000000000, 0.000000000000000000, 1.000000000000000000 ) ) ;
#3364 = FACE_OUTER_BOUND ( 'NONE', #266, .T. ) ;
#3365 = AXIS2_PLACEMENT_3D ( 'NONE', #7869, #9118, #12090 ) ;
#3366 = ADVANCED_FACE ( 'NONE', ( #9559 ), #8554, .T. ) ;
#3367 = CIRCLE ( 'NONE', #5570, 1.500000000000000222 ) ;
#3368 = CARTESIAN_POINT ( 'NONE',  ( -8.479748006907131597, 9.000000000000000000, 0.5864074857593127854 ) ) ;
#3369 = DIRECTION ( 'NONE',  ( -0.000000000000000000, -1.000000000000000000, -0.000000000000000000 ) ) ;
#3370 = VERTEX_POINT ( 'NONE', #3143 ) ;
#3371 = DIRECTION ( 'NONE',  ( 0.000000000000000000, 1.000000000000000000, 0.000000000000000000 ) ) ;
#3372 = ORIENTED_EDGE ( 'NONE', *, *, #12451, .F. ) ;
#3373 = ORIENTED_EDGE ( 'NONE', *, *, #3387, .T. ) ;
#3374 = ORIENTED_EDGE ( 'NONE', *, *, #11960, .T. ) ;
#3375 = CARTESIAN_POINT ( 'NONE',  ( 9.573149624528804580, 3.000000000000000000, -8.795158114916638681 ) ) ;
#3376 = EDGE_LOOP ( 'NONE', ( #3723, #6204, #237, #4823 ) ) ;
#3377 = CIRCLE ( 'NONE', #4701, 2.999999999999999112 ) ;
#3378 = AXIS2_PLACEMENT_3D ( 'NONE', #7576, #6542, #6474 ) ;
#3379 = ADVANCED_FACE ( 'NONE', ( #11564 ), #9620, .T. ) ;
#3380 = CARTESIAN_POINT ( 'NONE',  ( 31.00000000000000000, 3.000000000000000000, 3.999999998926329514 ) ) ;
#3381 = DIRECTION ( 'NONE',  ( 0.000000000000000000, 0.000000000000000000, 1.000000000000000000 ) ) ;
#3382 = FACE_OUTER_BOUND ( 'NONE', #7189, .T. ) ;
#3383 = CYLINDRICAL_SURFACE ( 'NONE', #7697, 8.500000000000000000 ) ;
#3384 = CARTESIAN_POINT ( 'NONE',  ( -2.414978278956346092, 0.000000000000000000, 13.33788847341978467 ) ) ;
#3385 = EDGE_CURVE ( 'NONE', #13469, #45, #8507, .T. ) ;
#3386 = DIRECTION ( 'NONE',  ( 0.000000000000000000, 0.000000000000000000, 1.000000000000000000 ) ) ;
#3387 = EDGE_CURVE ( 'NONE', #7832, #846, #5419, .T. ) ;
#3388 = CARTESIAN_POINT ( 'NONE',  ( -14.90895795148411374, 0.000000000000000000, -1.650143266773683726 ) ) ;
#3389 = B_SPLINE_SURFACE_WITH_KNOTS ( 'NONE', 3, 1, ( 
 ( #12837, #6354 ),
 ( #10759, #4359 ),
 ( #11863, #1397 ),
 ( #9793, #8747 ) ),
 .UNSPECIFIED., .F., .F., .F.,
 ( 4, 4 ),
 ( 2, 2 ),
 ( 0.1276832474596256706, 1.000000000000000000 ),
 ( 0.000000000000000000, 1.000000000000000000 ),
 .UNSPECIFIED. ) ;
#3390 = CARTESIAN_POINT ( 'NONE',  ( -3.835481108877868195, 9.000000000000000000, 5.554420281491219136 ) ) ;
#3391 = EDGE_LOOP ( 'NONE', ( #12627, #12308, #1470, #238 ) ) ;
#3392 = CARTESIAN_POINT ( 'NONE',  ( 0.000000000000000000, 0.000000000000000000, 0.000000000000000000 ) ) ;
#3393 = VECTOR ( 'NONE', #11992, 1000.000000000000000 ) ;
#3394 = ORIENTED_EDGE ( 'NONE', *, *, #6864, .F. ) ;
#3395 = CIRCLE ( 'NONE', #9988, 0.4000000000000000222 ) ;
#3396 = EDGE_LOOP ( 'NONE', ( #10299, #7048, #10491, #11825 ) ) ;
#3397 = EDGE_LOOP ( 'NONE', ( #12820, #7449, #235, #10058 ) ) ;
#3398 = CARTESIAN_POINT ( 'NONE',  ( 0.000000000000000000, 0.000000000000000000, 0.000000000000000000 ) ) ;
#3399 = AXIS2_PLACEMENT_3D ( 'NONE', #7040, #13239, #5796 ) ;
#3400 = CARTESIAN_POINT ( 'NONE',  ( 6.329356821613516537, 3.000000000000000000, -12.30759122141987305 ) ) ;
#3401 = DIRECTION ( 'NONE',  ( 1.000000000000000000, 0.000000000000000000, 0.000000000000000000 ) ) ;
#3402 = DIRECTION ( 'NONE',  ( 0.000000000000000000, 0.000000000000000000, 1.000000000000000000 ) ) ;
#3403 = DIRECTION ( 'NONE',  ( -0.000000000000000000, -1.000000000000000000, -0.000000000000000000 ) ) ;
#3404 = LINE ( 'NONE', #11877, #10147 ) ;
#3405 = CARTESIAN_POINT ( 'NONE',  ( 0.000000000000000000, 3.000000000000000000, 0.000000000000000000 ) ) ;
#3406 = ORIENTED_EDGE ( 'NONE', *, *, #7448, .F. ) ;
#3407 = PRESENTATION_LAYER_ASSIGNMENT (  '', '', ( #9790 ) ) ;
#3408 = VECTOR ( 'NONE', #9978, 1000.000000000000000 ) ;
#3409 = ORIENTED_EDGE ( 'NONE', *, *, #11372, .T. ) ;
#3410 = CARTESIAN_POINT ( 'NONE',  ( 3.893011711613070691, 3.000000000000000000, -12.40340517008307231 ) ) ;
#3411 = EDGE_CURVE ( 'NONE', #2737, #3746, #1022, .T. ) ;
#3412 = ORIENTED_EDGE ( 'NONE', *, *, #13142, .T. ) ;
#3413 = CARTESIAN_POINT ( 'NONE',  ( -10.15083332828461771, 3.000000000000000000, -29.86148447151320795 ) ) ;
#3414 = FACE_OUTER_BOUND ( 'NONE', #7967, .T. ) ;
#3415 = DIRECTION ( 'NONE',  ( 0.000000000000000000, 1.000000000000000000, 0.000000000000000000 ) ) ;
#3416 = DIRECTION ( 'NONE',  ( 0.000000000000000000, 0.000000000000000000, 1.000000000000000000 ) ) ;
#3417 = CARTESIAN_POINT ( 'NONE',  ( -7.798201703419567643, 0.000000000000000000, -27.99999999999999289 ) ) ;
#3418 = CARTESIAN_POINT ( 'NONE',  ( 8.158551673544282679, 0.000000000000000000, -8.922226997226884393 ) ) ;
#3419 = CARTESIAN_POINT ( 'NONE',  ( -7.494008246337227952, 0.000000000000000000, -11.63517940784355886 ) ) ;
#3420 = EDGE_LOOP ( 'NONE', ( #9911, #1329 ) ) ;
#3421 = ORIENTED_EDGE ( 'NONE', *, *, #4889, .F. ) ;
#3422 = EDGE_LOOP ( 'NONE', ( #1567, #287 ) ) ;
#3423 = AXIS2_PLACEMENT_3D ( 'NONE', #7612, #3078, #8374 ) ;
#3424 = VERTEX_POINT ( 'NONE', #196 ) ;
#3425 = DIRECTION ( 'NONE',  ( 0.000000000000000000, 0.000000000000000000, 1.000000000000000000 ) ) ;
#3426 = ORIENTED_EDGE ( 'NONE', *, *, #11384, .T. ) ;
#3427 = CARTESIAN_POINT ( 'NONE',  ( -5.452638258930639914, 0.000000000000000000, -13.97385902380748313 ) ) ;
#3428 = FILL_AREA_STYLE_COLOUR ( '', #7392 ) ;
#3429 = DIRECTION ( 'NONE',  ( 0.000000000000000000, 0.000000000000000000, -1.000000000000000000 ) ) ;
#3430 = DIRECTION ( 'NONE',  ( 0.000000000000000000, 1.000000000000000000, 0.000000000000000000 ) ) ;
#3431 =( REPRESENTATION_RELATIONSHIP ('NONE','NONE', #3798, #11353 ) REPRESENTATION_RELATIONSHIP_WITH_TRANSFORMATION ( #67 )SHAPE_REPRESENTATION_RELATIONSHIP( ) );
#3432 = CARTESIAN_POINT ( 'NONE',  ( -5.496871281090180972, 9.000000000000000000, 4.899765193453235135 ) ) ;
#3433 = CARTESIAN_POINT ( 'NONE',  ( 11.90209577080759296, 0.000000000000000000, -8.180229652970856691 ) ) ;
#3434 = ORIENTED_EDGE ( 'NONE', *, *, #7271, .T. ) ;
#3435 = CARTESIAN_POINT ( 'NONE',  ( 2.999999999999997335, 2.000000000000000000, -7.000000000000001776 ) ) ;
#3436 = ORIENTED_EDGE ( 'NONE', *, *, #888, .F. ) ;
#3437 = VERTEX_POINT ( 'NONE', #10522 ) ;
#3438 = EDGE_CURVE ( 'NONE', #11405, #9031, #9673, .T. ) ;
#3439 = PRODUCT_RELATED_PRODUCT_CATEGORY ( 'part', '', ( #9617 ) ) ;
#3440 = ORIENTED_EDGE ( 'NONE', *, *, #1788, .T. ) ;
#3441 = FACE_OUTER_BOUND ( 'NONE', #4881, .T. ) ;
#3442 = ORIENTED_EDGE ( 'NONE', *, *, #6934, .F. ) ;
#3443 = B_SPLINE_SURFACE_WITH_KNOTS ( 'NONE', 3, 1, ( 
 ( #3290, #12746 ),
 ( #5497, #155 ),
 ( #9577, #8285 ),
 ( #5370, #1959 ) ),
 .UNSPECIFIED., .F., .F., .F.,
 ( 4, 4 ),
 ( 2, 2 ),
 ( 0.000000000000000000, 0.8724294488011763438 ),
 ( 0.000000000000000000, 1.000000000000000000 ),
 .UNSPECIFIED. ) ;
#3444 = VERTEX_POINT ( 'NONE', #8571 ) ;
#3445 = CARTESIAN_POINT ( 'NONE',  ( -11.52330688609014686, 3.000000000000000000, -6.017756925049552841 ) ) ;
#3446 =( NAMED_UNIT ( * ) SI_UNIT ( $, .STERADIAN. ) SOLID_ANGLE_UNIT ( ) );
#3447 = LINE ( 'NONE', #2216, #8622 ) ;
#3448 = DIRECTION ( 'NONE',  ( 0.000000000000000000, 0.000000000000000000, 1.000000000000000000 ) ) ;
#3449 = CARTESIAN_POINT ( 'NONE',  ( 30.80713437936438126, 3.000000000000000000, 0.9994049933487144655 ) ) ;
#3450 = CARTESIAN_POINT ( 'NONE',  ( -8.922136023539609440, 3.000000000000000000, 8.158651161643900807 ) ) ;
#3451 = FACE_OUTER_BOUND ( 'NONE', #3396, .T. ) ;
#3452 = ORIENTED_EDGE ( 'NONE', *, *, #1203, .T. ) ;
#3453 = FACE_OUTER_BOUND ( 'NONE', #2568, .T. ) ;
#3454 = B_SPLINE_SURFACE_WITH_KNOTS ( 'NONE', 3, 1, ( 
 ( #3464, #5606 ),
 ( #3328, #439 ),
 ( #9808, #10771 ),
 ( #1413, #2373 ) ),
 .UNSPECIFIED., .F., .F., .F.,
 ( 4, 4 ),
 ( 2, 2 ),
 ( 0.000000000000000000, 0.8724294488011776760 ),
 ( 0.000000000000000000, 1.000000000000000000 ),
 .UNSPECIFIED. ) ;
#3455 = ADVANCED_FACE ( 'NONE', ( #4177 ), #12794, .T. ) ;
#3456 = EDGE_LOOP ( 'NONE', ( #11445, #7984, #6228, #8705 ) ) ;
#3457 = B_SPLINE_CURVE_WITH_KNOTS ( 'NONE', 3,
 ( #7627, #2526, #5551, #8647 ),
 .UNSPECIFIED., .F., .F.,
 ( 4, 4 ),
 ( 0.000000000000000000, 0.8452273900860258760 ),
 .UNSPECIFIED. ) ;
#3458 = VERTEX_POINT ( 'NONE', #10383 ) ;
#3459 = ORIENTED_EDGE ( 'NONE', *, *, #12071, .F. ) ;
#3460 = EDGE_CURVE ( 'NONE', #9662, #8736, #4395, .T. ) ;
#3461 = ADVANCED_FACE ( 'NONE', ( #9417 ), #3268, .F. ) ;
#3462 = DIRECTION ( 'NONE',  ( 0.000000000000000000, 0.000000000000000000, 1.000000000000000000 ) ) ;
#3463 = CARTESIAN_POINT ( 'NONE',  ( 8.914835885878215294, 0.000000000000000000, 11.11702303352197418 ) ) ;
#3464 = CARTESIAN_POINT ( 'NONE',  ( 6.749972395921142621, 9.000000000000000000, -0.01930425607464666612 ) ) ;
#3465 = DIRECTION ( 'NONE',  ( 1.000000000000000000, -3.469446951953610639E-15, 0.000000000000000000 ) ) ;
#3466 = CARTESIAN_POINT ( 'NONE',  ( -11.48836750521723893, 0.000000000000000000, 8.430890348300625448 ) ) ;
#3467 = CARTESIAN_POINT ( 'NONE',  ( 31.00000000000000000, 2.900000000000000355, 0.000000000000000000 ) ) ;
#3468 = EDGE_CURVE ( 'NONE', #8871, #4931, #10590, .T. ) ;
#3469 = ORIENTED_EDGE ( 'NONE', *, *, #6113, .F. ) ;
#3470 = ORIENTED_EDGE ( 'NONE', *, *, #9513, .F. ) ;
#3471 = CARTESIAN_POINT ( 'NONE',  ( 4.369710415961185035, 0.000000000000000000, 6.632530905044255576 ) ) ;
#3472 = CIRCLE ( 'NONE', #8104, 2.999999999999999112 ) ;
#3473 = EDGE_CURVE ( 'NONE', #10535, #2976, #2551, .T. ) ;
#3474 = EDGE_LOOP ( 'NONE', ( #978, #8024 ) ) ;
#3475 = CARTESIAN_POINT ( 'NONE',  ( -21.21140389626389577, 3.000000000000000000, -14.83930531255814955 ) ) ;
#3476 = PRODUCT_DEFINITION_SHAPE ( 'NONE', 'NONE',  #13608 ) ;
#3477 = CARTESIAN_POINT ( 'NONE',  ( -6.343077614891082128, 3.000000000000000000, -11.35348748332310720 ) ) ;
#3478 = B_SPLINE_CURVE_WITH_KNOTS ( 'NONE', 3,
 ( #3602, #7806, #13180, #2919 ),
 .UNSPECIFIED., .F., .F.,
 ( 4, 4 ),
 ( 0.1818127957067485756, 0.2112308727645026418 ),
 .UNSPECIFIED. ) ;
#3479 = LINE ( 'NONE', #9500, #730 ) ;
#3480 = FACE_BOUND ( 'NONE', #7468, .T. ) ;
#3481 = DIRECTION ( 'NONE',  ( -0.6923076923076904032, 0.000000000000000000, 0.7216024245882218802 ) ) ;
#3482 = FACE_OUTER_BOUND ( 'NONE', #112, .T. ) ;
#3483 = DIRECTION ( 'NONE',  ( 0.000000000000000000, 0.000000000000000000, -1.000000000000000000 ) ) ;
#3484 = ADVANCED_FACE ( 'NONE', ( #1617 ), #3900, .F. ) ;
#3485 = CARTESIAN_POINT ( 'NONE',  ( 0.000000000000000000, 9.000000000000000000, 0.000000000000000000 ) ) ;
#3486 = EDGE_LOOP ( 'NONE', ( #1951, #2929, #1610, #4440 ) ) ;
#3487 = ORIENTED_EDGE ( 'NONE', *, *, #6250, .F. ) ;
#3488 = ORIENTED_EDGE ( 'NONE', *, *, #4646, .T. ) ;
#3489 = EDGE_LOOP ( 'NONE', ( #7681, #1050, #2384, #10735 ) ) ;
#3490 = DIRECTION ( 'NONE',  ( 0.000000000000000000, 1.000000000000000000, -0.000000000000000000 ) ) ;
#3491 = VERTEX_POINT ( 'NONE', #12232 ) ;
#3492 = CARTESIAN_POINT ( 'NONE',  ( 7.500000000000003553, 3.000000000000000000, 13.39999999999999858 ) ) ;
#3493 = PRESENTATION_STYLE_ASSIGNMENT (( #13082 ) ) ;
#3494 = CARTESIAN_POINT ( 'NONE',  ( -2.830255545554292151, 3.000000000000000000, -12.68816982652971959 ) ) ;
#3495 = CARTESIAN_POINT ( 'NONE',  ( 0.000000000000000000, 2.900000000000000355, 0.000000000000000000 ) ) ;
#3496 = DIRECTION ( 'NONE',  ( -0.000000000000000000, -1.000000000000000000, -0.000000000000000000 ) ) ;
#3497 = CARTESIAN_POINT ( 'NONE',  ( 6.025412986832064277, 3.000000000000000000, -13.73660796332615597 ) ) ;
#3498 = VERTEX_POINT ( 'NONE', #11043 ) ;
#3499 = DIRECTION ( 'NONE',  ( 0.000000000000000000, 0.000000000000000000, 1.000000000000000000 ) ) ;
#3500 = VERTEX_POINT ( 'NONE', #12159 ) ;
#3501 = CIRCLE ( 'NONE', #13412, 1.499999999999997780 ) ;
#3502 = PRODUCT_DEFINITION_CONTEXT ( 'detailed design', #4143, 'design' ) ;
#3503 = VERTEX_POINT ( 'NONE', #9751 ) ;
#3504 = CARTESIAN_POINT ( 'NONE',  ( 12.00000000000001776, 8.000000000000000000, -10.00000000000000000 ) ) ;
#3505 = EDGE_LOOP ( 'NONE', ( #9109, #10052, #8894, #3426 ) ) ;
#3506 = ORIENTED_EDGE ( 'NONE', *, *, #707, .T. ) ;
#3507 = CARTESIAN_POINT ( 'NONE',  ( -14.90895795148411374, 3.000000000000000000, -1.650143266773683726 ) ) ;
#3508 = CIRCLE ( 'NONE', #10568, 1.499999999999999556 ) ;
#3509 = APPLICATION_CONTEXT ( 'automotive_design' ) ;
#3510 = DIRECTION ( 'NONE',  ( 0.000000000000000000, 0.000000000000000000, 1.000000000000000000 ) ) ;
#3511 = DIRECTION ( 'NONE',  ( 0.000000000000000000, 0.000000000000000000, -1.000000000000000000 ) ) ;
#3512 = AXIS2_PLACEMENT_3D ( 'NONE', #13116, #5808, #6522 ) ;
#3513 = EDGE_CURVE ( 'NONE', #11907, #12112, #7865, .T. ) ;
#3514 = CARTESIAN_POINT ( 'NONE',  ( 2.830255545554135832, 0.000000000000000000, -12.68816982652952596 ) ) ;
#3515 = FACE_OUTER_BOUND ( 'NONE', #5290, .T. ) ;
#3516 = FACE_OUTER_BOUND ( 'NONE', #7314, .T. ) ;
#3517 = ORIENTED_EDGE ( 'NONE', *, *, #13257, .T. ) ;
#3518 = LINE ( 'NONE', #2425, #5115 ) ;
#3519 = ORIENTED_EDGE ( 'NONE', *, *, #7769, .T. ) ;
#3520 = ORIENTED_EDGE ( 'NONE', *, *, #13438, .F. ) ;
#3521 = VECTOR ( 'NONE', #5004, 1000.000000000000000 ) ;
#3522 = VECTOR ( 'NONE', #13167, 1000.000000000000000 ) ;
#3523 = EDGE_LOOP ( 'NONE', ( #12464, #10452, #1777, #9402 ) ) ;
#3524 = DIRECTION ( 'NONE',  ( 0.000000000000000000, 0.000000000000000000, 1.000000000000000000 ) ) ;
#3525 = DIRECTION ( 'NONE',  ( -0.000000000000000000, -1.000000000000000000, -0.000000000000000000 ) ) ;
#3526 = EDGE_CURVE ( 'NONE', #11231, #9693, #257, .T. ) ;
#3527 = EDGE_CURVE ( 'NONE', #8040, #12695, #13421, .T. ) ;
#3528 = ITEM_DEFINED_TRANSFORMATION ( 'NONE', 'NONE', #1893,  #10007 ) ;
#3529 = ADVANCED_FACE ( 'NONE', ( #7557 ), #11827, .T. ) ;
#3530 = DIRECTION ( 'NONE',  ( 0.000000000000000000, 0.000000000000000000, 1.000000000000000000 ) ) ;
#3531 = AXIS2_PLACEMENT_3D ( 'NONE', #12529, #10372, #941 ) ;
#3532 = CARTESIAN_POINT ( 'NONE',  ( -14.16466328168010769, 0.000000000000000000, -1.557181465540673271 ) ) ;
#3533 = FACE_OUTER_BOUND ( 'NONE', #13189, .T. ) ;
#3534 = CIRCLE ( 'NONE', #686, 14.24999999999999822 ) ;
#3535 = CARTESIAN_POINT ( 'NONE',  ( -2.375523406013128280, 0.000000000000000000, 6.318179211409232998 ) ) ;
#3536 = ADVANCED_FACE ( 'NONE', ( #3342 ), #3029, .T. ) ;
#3537 = ORIENTED_EDGE ( 'NONE', *, *, #736, .T. ) ;
#3538 = VERTEX_POINT ( 'NONE', #12087 ) ;
#3539 = CARTESIAN_POINT ( 'NONE',  ( 10.18979803820051622, 0.000000000000000000, -6.506620931068703761 ) ) ;
#3540 = VECTOR ( 'NONE', #10293, 1000.000000000000000 ) ;
#3541 = ORIENTED_EDGE ( 'NONE', *, *, #7621, .T. ) ;
#3542 = CARTESIAN_POINT ( 'NONE',  ( 5.571433138827823761, 3.000000000000000000, 10.72973591378220704 ) ) ;
#3543 = CARTESIAN_POINT ( 'NONE',  ( -7.798201703419555209, 3.000000000000000000, -30.99999999999999289 ) ) ;
#3544 = ADVANCED_FACE ( 'NONE', ( #1283 ), #5545, .T. ) ;
#3545 = CARTESIAN_POINT ( 'NONE',  ( -8.922226997226788470, 3.000000000000000000, -8.158551673544387484 ) ) ;
#3546 = LINE ( 'NONE', #6657, #12791 ) ;
#3547 = LINE ( 'NONE', #5418, #4415 ) ;
#3548 = CIRCLE ( 'NONE', #11486, 0.1000000000000000472 ) ;
#3549 = CARTESIAN_POINT ( 'NONE',  ( 0.000000000000000000, 0.000000000000000000, 0.000000000000000000 ) ) ;
#3550 = EDGE_CURVE ( 'NONE', #7698, #11304, #6370, .T. ) ;
#3551 = AXIS2_PLACEMENT_3D ( 'NONE', #976, #6006, #11438 ) ;
#3552 = CARTESIAN_POINT ( 'NONE',  ( 3.469446951953614189E-15, 3.000000000000000000, -7.049999999999999822 ) ) ;
#3553 = CARTESIAN_POINT ( 'NONE',  ( -12.40340517008309185, 3.000000000000000000, -3.893011711613028947 ) ) ;
#3554 = VERTEX_POINT ( 'NONE', #12865 ) ;
#3555 = VERTEX_POINT ( 'NONE', #5880 ) ;
#3556 = EDGE_LOOP ( 'NONE', ( #3226, #5503, #9259, #1666 ) ) ;
#3557 = ORIENTED_EDGE ( 'NONE', *, *, #130, .F. ) ;
#3558 = CARTESIAN_POINT ( 'NONE',  ( 0.000000000000000000, 3.000000000000000000, 0.000000000000000000 ) ) ;
#3559 = EDGE_LOOP ( 'NONE', ( #1967, #12488, #7497, #5799 ) ) ;
#3560 = AXIS2_PLACEMENT_3D ( 'NONE', #2482, #9842, #6551 ) ;
#3561 = AXIS2_PLACEMENT_3D ( 'NONE', #9114, #7936, #3876 ) ;
#3562 = CIRCLE ( 'NONE', #7962, 9.250000000000000000 ) ;
#3563 = EDGE_CURVE ( 'NONE', #12771, #144, #171, .T. ) ;
#3564 = FACE_OUTER_BOUND ( 'NONE', #5744, .T. ) ;
#3565 = DIRECTION ( 'NONE',  ( 1.000000000000000000, 0.000000000000000000, 0.000000000000000000 ) ) ;
#3566 = B_SPLINE_SURFACE_WITH_KNOTS ( 'NONE', 3, 1, ( 
 ( #11574, #8514 ),
 ( #10530, #12734 ),
 ( #4329, #3276 ),
 ( #3350, #7631 ) ),
 .UNSPECIFIED., .F., .F., .F.,
 ( 4, 4 ),
 ( 2, 2 ),
 ( 0.000000000000000000, 0.5855695330273008592 ),
 ( 0.000000000000000000, 1.000000000000000000 ),
 .UNSPECIFIED. ) ;
#3567 = CARTESIAN_POINT ( 'NONE',  ( -10.98198414889942676, 3.000000000000000000, -9.379342464487661957 ) ) ;
#3568 = FACE_BOUND ( 'NONE', #12002, .T. ) ;
#3569 = CARTESIAN_POINT ( 'NONE',  ( 13.11311062740304401, 3.000000000000000000, -1.563624455674628377 ) ) ;
#3570 = EDGE_LOOP ( 'NONE', ( #1870, #7741, #6296, #2143 ) ) ;
#3571 = AXIS2_PLACEMENT_3D ( 'NONE', #7968, #4947, #11208 ) ;
#3572 = FACE_OUTER_BOUND ( 'NONE', #8262, .T. ) ;
#3573 = AXIS2_PLACEMENT_3D ( 'NONE', #1766, #6106, #8160 ) ;
#3574 = AXIS2_PLACEMENT_3D ( 'NONE', #1550, #12166, #5741 ) ;
#3575 = ORIENTED_EDGE ( 'NONE', *, *, #12017, .T. ) ;
#3576 = VERTEX_POINT ( 'NONE', #4915 ) ;
#3577 = LINE ( 'NONE', #4549, #1819 ) ;
#3578 = ORIENTED_EDGE ( 'NONE', *, *, #8334, .F. ) ;
#3579 = EDGE_CURVE ( 'NONE', #2082, #13415, #3666, .T. ) ;
#3580 = ORIENTED_EDGE ( 'NONE', *, *, #9398, .T. ) ;
#3581 = EDGE_CURVE ( 'NONE', #5694, #7353, #11439, .T. ) ;
#3582 = DIRECTION ( 'NONE',  ( -1.000000000000000000, 3.491481338843133355E-15, 2.602085213965210149E-16 ) ) ;
#3583 = CIRCLE ( 'NONE', #9091, 6.750000000000001776 ) ;
#3584 = AXIS2_PLACEMENT_3D ( 'NONE', #11256, #722, #5813 ) ;
#3585 = AXIS2_PLACEMENT_3D ( 'NONE', #7025, #2, #6257 ) ;
#3586 = CARTESIAN_POINT ( 'NONE',  ( -13.03533457366735426, 0.000000000000000000, -6.217402469309218027 ) ) ;
#3587 = CARTESIAN_POINT ( 'NONE',  ( 0.5400000000008007284, 0.000000000000000000, 12.07793442604883793 ) ) ;
#3588 = CARTESIAN_POINT ( 'NONE',  ( 0.000000000000000000, 9.000000000000000000, 0.000000000000000000 ) ) ;
#3589 = CARTESIAN_POINT ( 'NONE',  ( -14.20034848914876235, 0.000000000000000000, -2.631756770590732764 ) ) ;
#3590 = CARTESIAN_POINT ( 'NONE',  ( 0.000000000000000000, 0.000000000000000000, 0.000000000000000000 ) ) ;
#3591 = EDGE_LOOP ( 'NONE', ( #3024, #5472, #1836, #5702 ) ) ;
#3592 = PLANE ( 'NONE',  #2247 ) ;
#3593 = ORIENTED_EDGE ( 'NONE', *, *, #10720, .F. ) ;
#3594 = VECTOR ( 'NONE', #1348, 1000.000000000000000 ) ;
#3595 = PRODUCT_DEFINITION_SHAPE ( 'NONE', 'NONE',  #13606 ) ;
#3596 = VERTEX_POINT ( 'NONE', #5474 ) ;
#3597 = CIRCLE ( 'NONE', #2074, 1.500000000000000222 ) ;
#3598 = VERTEX_POINT ( 'NONE', #9682 ) ;
#3599 = CARTESIAN_POINT ( 'NONE',  ( -6.749999880766614169, 1.734723475976807094E-15, -0.001268720102703522860 ) ) ;
#3600 = CARTESIAN_POINT ( 'NONE',  ( 4.056222772158357692, 3.000000000000000000, -12.16218796965919680 ) ) ;
#3601 = CARTESIAN_POINT ( 'NONE',  ( -8.180229652970899323, 0.000000000000000000, -11.90209577080756276 ) ) ;
#3602 = CARTESIAN_POINT ( 'NONE',  ( -12.40340517008309185, 0.000000000000000000, -3.893011711613028947 ) ) ;
#3603 = B_SPLINE_CURVE_WITH_KNOTS ( 'NONE', 3,
 ( #10654, #1482, #246, #5533 ),
 .UNSPECIFIED., .F., .F.,
 ( 4, 4 ),
 ( 0.1547128134717859205, 1.000000000000000000 ),
 .UNSPECIFIED. ) ;
#3604 = ITEM_DEFINED_TRANSFORMATION ( 'NONE', 'NONE', #9137,  #10007 ) ;
#3605 = AXIS2_PLACEMENT_3D ( 'NONE', #3757, #7885, #5686 ) ;
#3606 = CARTESIAN_POINT ( 'NONE',  ( -7.939678587550617728, 0.000000000000000000, 0.2057875656132798770 ) ) ;
#3607 = CARTESIAN_POINT ( 'NONE',  ( 6.000000000000008882, 0.000000000000000000, 27.00000000000000000 ) ) ;
#3608 = CARTESIAN_POINT ( 'NONE',  ( -10.18987059060247624, 3.000000000000000000, -6.506507307819711095 ) ) ;
#3609 = CIRCLE ( 'NONE', #9567, 0.09999999999999982514 ) ;
#3610 = DIRECTION ( 'NONE',  ( 0.000000000000000000, 0.000000000000000000, -1.000000000000000000 ) ) ;
#3611 = EDGE_LOOP ( 'NONE', ( #178, #2274, #10473, #11739 ) ) ;
#3612 = EDGE_LOOP ( 'NONE', ( #6342, #8474, #219, #5201 ) ) ;
#3613 = ADVANCED_FACE ( 'NONE', ( #3414 ), #2386, .F. ) ;
#3614 = PRESENTATION_LAYER_ASSIGNMENT (  '', '', ( #5378 ) ) ;
#3615 = VECTOR ( 'NONE', #4496, 1000.000000000000000 ) ;
#3616 = ORIENTED_EDGE ( 'NONE', *, *, #8932, .T. ) ;
#3617 = CYLINDRICAL_SURFACE ( 'NONE', #11074, 1.500000000000000222 ) ;
#3618 = CYLINDRICAL_SURFACE ( 'NONE', #4498, 12.08999999999737440 ) ;
#3619 = FACE_OUTER_BOUND ( 'NONE', #12882, .T. ) ;
#3620 = DIRECTION ( 'NONE',  ( -0.000000000000000000, -1.000000000000000000, -0.000000000000000000 ) ) ;
#3621 = CARTESIAN_POINT ( 'NONE',  ( 11.48836750521724070, 0.000000000000000000, -8.430890348300621895 ) ) ;
#3622 = AXIS2_PLACEMENT_3D ( 'NONE', #7393, #12759, #227 ) ;
#3623 = DIRECTION ( 'NONE',  ( -0.000000000000000000, -1.000000000000000000, -0.000000000000000000 ) ) ;
#3624 = CARTESIAN_POINT ( 'NONE',  ( -7.235926821844430812, 9.000000000000000000, 4.459973433655439301 ) ) ;
#3625 = DIRECTION ( 'NONE',  ( -0.000000000000000000, -1.000000000000000000, -0.000000000000000000 ) ) ;
#3626 = ORIENTED_EDGE ( 'NONE', *, *, #192, .F. ) ;
#3627 = ADVANCED_FACE ( 'NONE', ( #11254 ), #992, .T. ) ;
#3628 = ORIENTED_EDGE ( 'NONE', *, *, #4378, .F. ) ;
#3629 = EDGE_CURVE ( 'NONE', #3437, #2462, #7237, .T. ) ;
#3630 = ORIENTED_EDGE ( 'NONE', *, *, #10402, .F. ) ;
#3631 = CARTESIAN_POINT ( 'NONE',  ( 31.00000000000000000, -8.809142651444723526E-17, 1.600000000000004086 ) ) ;
#3632 = ORIENTED_EDGE ( 'NONE', *, *, #11103, .F. ) ;
#3633 = EDGE_CURVE ( 'NONE', #7408, #6519, #9244, .T. ) ;
#3634 = EDGE_CURVE ( 'NONE', #10193, #7606, #6808, .T. ) ;
#3635 = LINE ( 'NONE', #347, #657 ) ;
#3636 = DIRECTION ( 'NONE',  ( -0.000000000000000000, -1.000000000000000000, -0.000000000000000000 ) ) ;
#3637 = DIRECTION ( 'NONE',  ( -0.000000000000000000, -1.000000000000000000, 0.000000000000000000 ) ) ;
#3638 = CARTESIAN_POINT ( 'NONE',  ( 6.509732753943064054, 0.000000000000000000, -3.441899519755141412 ) ) ;
#3639 = LINE ( 'NONE', #7838, #1822 ) ;
#3640 = CARTESIAN_POINT ( 'NONE',  ( -1.604252589105052307, 9.000000000000000000, -8.347237484961700815 ) ) ;
#3641 = ORIENTED_EDGE ( 'NONE', *, *, #13521, .T. ) ;
#3642 = FACE_OUTER_BOUND ( 'NONE', #3489, .T. ) ;
#3643 = EDGE_CURVE ( 'NONE', #2068, #1584, #7907, .T. ) ;
#3644 = ORIENTED_EDGE ( 'NONE', *, *, #4976, .F. ) ;
#3645 = UNCERTAINTY_MEASURE_WITH_UNIT (LENGTH_MEASURE( 1.000000000000000082E-05 ), #12139, 'distance_accuracy_value', 'NONE');
#3646 = ORIENTED_EDGE ( 'NONE', *, *, #2669, .F. ) ;
#3647 = CARTESIAN_POINT ( 'NONE',  ( 1.836970198721030181E-16, 0.000000000000000000, 1.500000000000000222 ) ) ;
#3648 = ORIENTED_EDGE ( 'NONE', *, *, #10020, .F. ) ;
#3649 = VERTEX_POINT ( 'NONE', #7257 ) ;
#3650 = CARTESIAN_POINT ( 'NONE',  ( 0.000000000000000000, 0.000000000000000000, 0.000000000000000000 ) ) ;
#3651 = CARTESIAN_POINT ( 'NONE',  ( -6.217402469309367241, 3.000000000000000000, -13.03533457366727610 ) ) ;
#3652 = CARTESIAN_POINT ( 'NONE',  ( -5.065227977808753224, 0.000000000000000000, -4.461610195077944319 ) ) ;
#3653 = DIRECTION ( 'NONE',  ( 0.000000000000000000, 0.000000000000000000, 1.000000000000000000 ) ) ;
#3654 = FACE_OUTER_BOUND ( 'NONE', #12458, .T. ) ;
#3655 = ORIENTED_EDGE ( 'NONE', *, *, #10658, .T. ) ;
#3656 = FACE_BOUND ( 'NONE', #5012, .T. ) ;
#3657 = EDGE_CURVE ( 'NONE', #12875, #1362, #8214, .T. ) ;
#3658 = ORIENTED_EDGE ( 'NONE', *, *, #1478, .T. ) ;
#3659 = EDGE_CURVE ( 'NONE', #5441, #10694, #12554, .T. ) ;
#3660 = ORIENTED_EDGE ( 'NONE', *, *, #6391, .T. ) ;
#3661 = ORIENTED_EDGE ( 'NONE', *, *, #6558, .T. ) ;
#3662 = EDGE_CURVE ( 'NONE', #12096, #6347, #8082, .T. ) ;
#3663 = CARTESIAN_POINT ( 'NONE',  ( 0.000000000000000000, 0.09999999999999982514, 1.399999999999999911 ) ) ;
#3664 = DIRECTION ( 'NONE',  ( 0.000000000000000000, 0.000000000000000000, 1.000000000000000000 ) ) ;
#3665 = CARTESIAN_POINT ( 'NONE',  ( -14.39763212228012534, 3.000000000000000000, 1.133238802859812155 ) ) ;
#3666 = LINE ( 'NONE', #4841, #5489 ) ;
#3667 = CARTESIAN_POINT ( 'NONE',  ( -4.679611352264966051, 9.000000000000000000, -6.417326716594978997 ) ) ;
#3668 = CONTEXT_DEPENDENT_SHAPE_REPRESENTATION ( #10492, #9975 ) ;
#3669 = CARTESIAN_POINT ( 'NONE',  ( 7.248474140376191421, 0.000000000000000000, 4.439552076088042476 ) ) ;
#3670 = CARTESIAN_POINT ( 'NONE',  ( -8.795158114916672432, 0.000000000000000000, -9.573149624528774382 ) ) ;
#3671 = DIRECTION ( 'NONE',  ( 0.9288742131985401329, 0.000000000000000000, -0.3703953240185316464 ) ) ;
#3672 = PLANE ( 'NONE',  #9747 ) ;
#3673 = CARTESIAN_POINT ( 'NONE',  ( 0.000000000000000000, 3.000000000000000000, 0.000000000000000000 ) ) ;
#3674 = ORIENTED_EDGE ( 'NONE', *, *, #12150, .T. ) ;
#3675 = ORIENTED_EDGE ( 'NONE', *, *, #2678, .T. ) ;
#3676 = B_SPLINE_SURFACE_WITH_KNOTS ( 'NONE', 3, 1, ( 
 ( #3084, #9367 ),
 ( #13429, #4121 ),
 ( #3985, #12541 ),
 ( #8181, #11495 ) ),
 .UNSPECIFIED., .F., .F., .F.,
 ( 4, 4 ),
 ( 2, 2 ),
 ( 0.1547128134717859205, 1.000000000000000000 ),
 ( 0.000000000000000000, 1.000000000000000000 ),
 .UNSPECIFIED. ) ;
#3677 = ORIENTED_EDGE ( 'NONE', *, *, #1638, .F. ) ;
#3678 = DIRECTION ( 'NONE',  ( 0.000000000000000000, 0.000000000000000000, 1.000000000000000000 ) ) ;
#3679 = CARTESIAN_POINT ( 'NONE',  ( 41.29994854050690378, 3.000000000000000000, -5.141175130212632283 ) ) ;
#3680 = CARTESIAN_POINT ( 'NONE',  ( 20.03271148078819408, 3.000000000000000000, -5.075121771833452478 ) ) ;
#3681 = CARTESIAN_POINT ( 'NONE',  ( 31.00000000000000000, 3.000000000000000000, 3.999999998926329514 ) ) ;
#3682 = CARTESIAN_POINT ( 'NONE',  ( -2.161962830978783057, 3.000000000000000000, -14.08504230442586369 ) ) ;
#3683 = ADVANCED_FACE ( 'NONE', ( #5117 ), #7197, .T. ) ;
#3684 = LINE ( 'NONE', #1494, #7574 ) ;
#3685 = CARTESIAN_POINT ( 'NONE',  ( 3.188443874008702661, 3.000000000000000000, -12.60833581801614578 ) ) ;
#3686 = LINE ( 'NONE', #6789, #13503 ) ;
#3687 = ORIENTED_EDGE ( 'NONE', *, *, #11709, .T. ) ;
#3688 = ORIENTED_EDGE ( 'NONE', *, *, #7105, .T. ) ;
#3689 = ORIENTED_EDGE ( 'NONE', *, *, #7911, .T. ) ;
#3690 = CARTESIAN_POINT ( 'NONE',  ( 0.000000000000000000, 0.000000000000000000, 0.000000000000000000 ) ) ;
#3691 = VERTEX_POINT ( 'NONE', #12374 ) ;
#3692 = DIRECTION ( 'NONE',  ( 0.000000000000000000, 0.000000000000000000, 1.000000000000000000 ) ) ;
#3693 = CARTESIAN_POINT ( 'NONE',  ( 33.92696780347524310, 32.33135765298362685, 14.10964106095043569 ) ) ;
#3694 = EDGE_CURVE ( 'NONE', #8654, #5917, #5278, .T. ) ;
#3695 = CARTESIAN_POINT ( 'NONE',  ( 6.554160776451332104, 9.000000000000000000, -1.614148852004323231 ) ) ;
#3696 = CARTESIAN_POINT ( 'NONE',  ( 5.958322434183388694, 0.000000000000000000, -6.062045345451230638 ) ) ;
#3697 = ADVANCED_FACE ( 'NONE', ( #8341 ), #2843, .T. ) ;
#3698 = FACE_OUTER_BOUND ( 'NONE', #9826, .T. ) ;
#3699 = CARTESIAN_POINT ( 'NONE',  ( -2.604531154829235362, 3.000000000000000000, -11.80612203322752585 ) ) ;
#3700 = AXIS2_PLACEMENT_3D ( 'NONE', #8194, #12426, #7991 ) ;
#3701 = CARTESIAN_POINT ( 'NONE',  ( 31.00000000000000000, 0.09999999999999982514, -1.600000000000004086 ) ) ;
#3702 = VERTEX_POINT ( 'NONE', #853 ) ;
#3703 = EDGE_CURVE ( 'NONE', #1162, #2665, #8683, .T. ) ;
#3704 = CARTESIAN_POINT ( 'NONE',  ( -6.970598036433426792, 3.000000000000000000, -10.97318381393771780 ) ) ;
#3705 = EDGE_CURVE ( 'NONE', #10836, #937, #882, .T. ) ;
#3706 = ORIENTED_EDGE ( 'NONE', *, *, #8465, .T. ) ;
#3707 = ORIENTED_EDGE ( 'NONE', *, *, #6449, .F. ) ;
#3708 = CARTESIAN_POINT ( 'NONE',  ( -7.712570079660889810, 0.000000000000000000, 11.14709020439930320 ) ) ;
#3709 = EDGE_LOOP ( 'NONE', ( #13077, #1222, #9830, #691 ) ) ;
#3710 = ORIENTED_EDGE ( 'NONE', *, *, #5809, .T. ) ;
#3711 = CYLINDRICAL_SURFACE ( 'NONE', #7428, 3.000000000000000000 ) ;
#3712 =( NAMED_UNIT ( * ) PLANE_ANGLE_UNIT ( ) SI_UNIT ( $, .RADIAN. ) );
#3713 = CARTESIAN_POINT ( 'NONE',  ( -11.52662650599092409, 3.000000000000000000, 3.647599401157420651 ) ) ;
#3714 = EDGE_CURVE ( 'NONE', #12719, #6705, #7130, .T. ) ;
#3715 = CARTESIAN_POINT ( 'NONE',  ( 0.000000000000000000, 0.000000000000000000, 0.000000000000000000 ) ) ;
#3716 = B_SPLINE_CURVE_WITH_KNOTS ( 'NONE', 2,
 ( #11109, #3796, #7797 ),
 .UNSPECIFIED., .F., .F.,
 ( 3, 3 ),
 ( 0.000000000000000000, 1.000000000000000000 ),
 .UNSPECIFIED. ) ;
#3717 = CARTESIAN_POINT ( 'NONE',  ( 31.00000000000000000, 2.900000000000000355, 0.000000000000000000 ) ) ;
#3718 = CARTESIAN_POINT ( 'NONE',  ( -5.065227977808755000, 0.000000000000000000, -4.461610195077942542 ) ) ;
#3719 = CARTESIAN_POINT ( 'NONE',  ( -0.7901945867173586491, 0.000000000000000000, -12.78643498603818074 ) ) ;
#3720 = VERTEX_POINT ( 'NONE', #6022 ) ;
#3721 = DIRECTION ( 'NONE',  ( -0.000000000000000000, -1.000000000000000000, -0.000000000000000000 ) ) ;
#3722 = EDGE_CURVE ( 'NONE', #9128, #6683, #6597, .T. ) ;
#3723 = ORIENTED_EDGE ( 'NONE', *, *, #2906, .F. ) ;
#3724 = ORIENTED_EDGE ( 'NONE', *, *, #10708, .T. ) ;
#3725 = ORIENTED_EDGE ( 'NONE', *, *, #432, .F. ) ;
#3726 = VECTOR ( 'NONE', #3754, 1000.000000000000000 ) ;
#3727 = VECTOR ( 'NONE', #13392, 1000.000000000000000 ) ;
#3728 = CARTESIAN_POINT ( 'NONE',  ( -13.82336506795094522, 3.000000000000000000, -0.6724118135761603110 ) ) ;
#3729 = CARTESIAN_POINT ( 'NONE',  ( 0.000000000000000000, 3.000000000000000000, 0.000000000000000000 ) ) ;
#3730 = CARTESIAN_POINT ( 'NONE',  ( 30.66173999750687784, 3.000000000000000000, 0.01003121477750366919 ) ) ;
#3731 = EDGE_CURVE ( 'NONE', #6099, #8207, #4986, .T. ) ;
#3732 = DIRECTION ( 'NONE',  ( -0.000000000000000000, -1.000000000000000000, -0.000000000000000000 ) ) ;
#3733 = ADVANCED_FACE ( 'NONE', ( #3940 ), #8143, .T. ) ;
#3734 = DIRECTION ( 'NONE',  ( -0.7772490812545826966, 0.000000000000000000, -0.6291930273683166153 ) ) ;
#3735 = CONTEXT_DEPENDENT_SHAPE_REPRESENTATION ( #6521, #1064 ) ;
#3736 = DIRECTION ( 'NONE',  ( 0.000000000000000000, 1.000000000000000000, -0.000000000000000000 ) ) ;
#3737 = CARTESIAN_POINT ( 'NONE',  ( 0.000000000000000000, 0.000000000000000000, 0.000000000000000000 ) ) ;
#3738 = DIRECTION ( 'NONE',  ( -0.000000000000000000, -1.000000000000000000, 0.000000000000000000 ) ) ;
#3739 = PLANE ( 'NONE',  #6891 ) ;
#3740 = FACE_OUTER_BOUND ( 'NONE', #9235, .T. ) ;
#3741 = AXIS2_PLACEMENT_3D ( 'NONE', #11008, #3247, #3312 ) ;
#3742 = VERTEX_POINT ( 'NONE', #7395 ) ;
#3743 = ORIENTED_EDGE ( 'NONE', *, *, #9108, .T. ) ;
#3744 = B_SPLINE_CURVE_WITH_KNOTS ( 'NONE', 3,
 ( #4877, #2812, #9472, #9214 ),
 .UNSPECIFIED., .F., .F.,
 ( 4, 4 ),
 ( 0.000000000000000000, 0.8452273900860258760 ),
 .UNSPECIFIED. ) ;
#3745 = ADVANCED_BREP_SHAPE_REPRESENTATION ( '', ( #8567, #10007 ), #10678 ) ;
#3746 = VERTEX_POINT ( 'NONE', #1192 ) ;
#3747 = LINE ( 'NONE', #13269, #5349 ) ;
#3748 = CARTESIAN_POINT ( 'NONE',  ( 6.506620931068708202, 3.000000000000000000, 10.18979803820052155 ) ) ;
#3749 = AXIS2_PLACEMENT_3D ( 'NONE', #8715, #3347, #7686 ) ;
#3750 = B_SPLINE_SURFACE_WITH_KNOTS ( 'NONE', 3, 1, ( 
 ( #10039, #2740 ),
 ( #2870, #4742 ),
 ( #9893, #468 ),
 ( #3902, #8990 ) ),
 .UNSPECIFIED., .F., .F., .F.,
 ( 4, 4 ),
 ( 2, 2 ),
 ( 0.6363612417694253232, 0.6657793188270956231 ),
 ( 0.000000000000000000, 1.000000000000000000 ),
 .UNSPECIFIED. ) ;
#3751 = AXIS2_PLACEMENT_3D ( 'NONE', #11289, #5909, #8250 ) ;
#3752 = EDGE_CURVE ( 'NONE', #4948, #175, #6417, .T. ) ;
#3753 = DIRECTION ( 'NONE',  ( -0.000000000000000000, -1.000000000000000000, -0.000000000000000000 ) ) ;
#3754 = DIRECTION ( 'NONE',  ( -0.000000000000000000, -1.000000000000000000, -0.000000000000000000 ) ) ;
#3755 = CARTESIAN_POINT ( 'NONE',  ( 0.000000000000000000, 3.000000000000000000, -1.500000000000000222 ) ) ;
#3756 = DIRECTION ( 'NONE',  ( -0.000000000000000000, -1.000000000000000000, -0.000000000000000000 ) ) ;
#3757 = CARTESIAN_POINT ( 'NONE',  ( 0.000000000000000000, 3.000000000000000000, 0.000000000000000000 ) ) ;
#3758 = CARTESIAN_POINT ( 'NONE',  ( -10.72973591378220348, 3.000000000000000000, 5.571433138827830867 ) ) ;
#3759 = VERTEX_POINT ( 'NONE', #8682 ) ;
#3760 = VECTOR ( 'NONE', #2638, 1000.000000000000000 ) ;
#3761 = VERTEX_POINT ( 'NONE', #11730 ) ;
#3762 = VECTOR ( 'NONE', #3403, 1000.000000000000000 ) ;
#3763 = ORIENTED_EDGE ( 'NONE', *, *, #10239, .F. ) ;
#3764 = CYLINDRICAL_SURFACE ( 'NONE', #11061, 8.500000000000000000 ) ;
#3765 = ORIENTED_EDGE ( 'NONE', *, *, #12543, .F. ) ;
#3766 = CARTESIAN_POINT ( 'NONE',  ( -5.733772933379472470, 3.000000000000000000, 13.04554897075799502 ) ) ;
#3767 = CARTESIAN_POINT ( 'NONE',  ( 15.17696780347061214, 31.33135765298362330, 35.00042399990212516 ) ) ;
#3768 = CIRCLE ( 'NONE', #1137, 12.00000000000000000 ) ;
#3769 = DIRECTION ( 'NONE',  ( -0.000000000000000000, -1.000000000000000000, -0.000000000000000000 ) ) ;
#3770 = CARTESIAN_POINT ( 'NONE',  ( 12.08646469655232636, 3.000000000000000000, -8.883544964652022813 ) ) ;
#3771 = CARTESIAN_POINT ( 'NONE',  ( -6.524296280129988190, 9.000000000000000000, -3.413039245436654490 ) ) ;
#3772 = DIRECTION ( 'NONE',  ( -0.000000000000000000, -1.000000000000000000, 0.000000000000000000 ) ) ;
#3773 = CARTESIAN_POINT ( 'NONE',  ( -1.161309641800940540, 9.000000000000000000, -7.856984441350959969 ) ) ;
#3774 = VERTEX_POINT ( 'NONE', #6350 ) ;
#3775 = DIRECTION ( 'NONE',  ( -0.000000000000000000, -1.000000000000000000, -0.000000000000000000 ) ) ;
#3776 = ORIENTED_EDGE ( 'NONE', *, *, #2615, .T. ) ;
#3777 = UNCERTAINTY_MEASURE_WITH_UNIT (LENGTH_MEASURE( 1.000000000000000082E-05 ), #12389, 'distance_accuracy_value', 'NONE');
#3778 = VECTOR ( 'NONE', #60, 1000.000000000000000 ) ;
#3779 = ORIENTED_EDGE ( 'NONE', *, *, #1122, .F. ) ;
#3780 = CARTESIAN_POINT ( 'NONE',  ( -2.264806262022998062, 3.000000000000000000, -14.82803603298499340 ) ) ;
#3781 = AXIS2_PLACEMENT_3D ( 'NONE', #475, #3496, #8732 ) ;
#3782 = EDGE_CURVE ( 'NONE', #13024, #5187, #12789, .T. ) ;
#3783 = ORIENTED_EDGE ( 'NONE', *, *, #10040, .T. ) ;
#3784 = FACE_OUTER_BOUND ( 'NONE', #6403, .T. ) ;
#3785 = ORIENTED_EDGE ( 'NONE', *, *, #3662, .T. ) ;
#3786 = CARTESIAN_POINT ( 'NONE',  ( 51.38094353598858532, 3.000000000000000000, -3.436371243710653722 ) ) ;
#3787 = PLANE ( 'NONE',  #10165 ) ;
#3788 = DIRECTION ( 'NONE',  ( -0.000000000000000000, -1.000000000000000000, -0.000000000000000000 ) ) ;
#3789 = VECTOR ( 'NONE', #6193, 1000.000000000000227 ) ;
#3790 = CARTESIAN_POINT ( 'NONE',  ( 8.795158114916441505, 0.000000000000000000, -9.573149624528689117 ) ) ;
#3791 = VECTOR ( 'NONE', #3047, 1000.000000000000114 ) ;
#3792 = VECTOR ( 'NONE', #10358, 1000.000000000000000 ) ;
#3793 = CARTESIAN_POINT ( 'NONE',  ( -13.04554897075799680, 0.000000000000000000, -5.733772933379471581 ) ) ;
#3794 = LINE ( 'NONE', #2624, #10670 ) ;
#3795 = EDGE_LOOP ( 'NONE', ( #2500, #8434, #8534, #11867 ) ) ;
#3796 = CARTESIAN_POINT ( 'NONE',  ( -13.86115248177182835, 3.000000000000000000, -5.741477348071267528 ) ) ;
#3797 = EDGE_LOOP ( 'NONE', ( #13188, #12752, #9385, #10487 ) ) ;
#3798 = SHAPE_REPRESENTATION ( 'MAT-047', ( #1020, #10472, #6283, #9137, #1893, #354, #8045, #3198, #2110, #9803, #3863, #7181, #12252, #8917, #4098, #805, #11359, #3207, #5406, #9378, #10908, #1234, #10480, #4533, #6512, #3423 ), #6721 ) ;
#3799 = VERTEX_POINT ( 'NONE', #10757 ) ;
#3800 = CARTESIAN_POINT ( 'NONE',  ( 6.749972395921142621, 9.000000000000000000, -0.01930425607464712062 ) ) ;
#3801 = EDGE_CURVE ( 'NONE', #7249, #2378, #10116, .T. ) ;
#3802 = ORIENTED_EDGE ( 'NONE', *, *, #10438, .T. ) ;
#3803 = CIRCLE ( 'NONE', #3571, 1.000000000000000888 ) ;
#3804 = CIRCLE ( 'NONE', #11511, 2.500000000000000444 ) ;
#3805 = AXIS2_PLACEMENT_3D ( 'NONE', #1045, #10339, #5241 ) ;
#3806 = CARTESIAN_POINT ( 'NONE',  ( -7.363095878837111030, -1.694065894508600678E-18, 0.009895496992605581216 ) ) ;
#3807 = EDGE_CURVE ( 'NONE', #9307, #1347, #5941, .T. ) ;
#3808 = DIRECTION ( 'NONE',  ( 0.000000000000000000, 0.000000000000000000, 1.000000000000000000 ) ) ;
#3809 = ADVANCED_FACE ( 'NONE', ( #9653 ), #7656, .F. ) ;
#3810 = CARTESIAN_POINT ( 'NONE',  ( 12.21000000000000796, 0.000000000000000000, 0.2208617994340217328 ) ) ;
#3811 = CARTESIAN_POINT ( 'NONE',  ( -13.00394681030572208, 0.000000000000000000, -0.1834665838397169235 ) ) ;
#3812 = LINE ( 'NONE', #9932, #3960 ) ;
#3813 = CARTESIAN_POINT ( 'NONE',  ( 0.000000000000000000, 3.000000000000000000, 0.000000000000000000 ) ) ;
#3814 = CARTESIAN_POINT ( 'NONE',  ( 2.719999999999997087, 2.000000000000000000, -6.000000000000000000 ) ) ;
#3815 = CYLINDRICAL_SURFACE ( 'NONE', #4205, 1.499999999999999556 ) ;
#3816 = B_SPLINE_CURVE_WITH_KNOTS ( 'NONE', 3,
 ( #8064, #951, #5859, #7354 ),
 .UNSPECIFIED., .F., .F.,
 ( 4, 4 ),
 ( 0.1547128134717859205, 1.000000000000000000 ),
 .UNSPECIFIED. ) ;
#3817 = AXIS2_PLACEMENT_3D ( 'NONE', #10664, #10589, #2326 ) ;
#3818 = CARTESIAN_POINT ( 'NONE',  ( -8.222660081691577361, 3.000000000000000000, -8.549999999999998934 ) ) ;
#3819 = CARTESIAN_POINT ( 'NONE',  ( 0.000000000000000000, 0.09999999999999982514, 0.000000000000000000 ) ) ;
#3820 = AXIS2_PLACEMENT_3D ( 'NONE', #243, #8825, #3402 ) ;
#3821 = CIRCLE ( 'NONE', #10860, 12.08999999999737440 ) ;
#3822 = VERTEX_POINT ( 'NONE', #2289 ) ;
#3823 = EDGE_LOOP ( 'NONE', ( #4203, #3743, #2866, #1068, #2770, #7948, #12136, #9629, #9158, #8873, #8668, #4928, #5204, #2273, #9207, #4995, #564, #4909, #11246, #5690, #2819, #6689, #10302, #9159, #2048, #10641, #1324, #12710, #2757, #9330, #6734, #4744, #7015, #6628, #1485, #4025, #5914, #12033, #5957, #400, #1292, #5107, #4531, #5439, #8975, #3487, #1906, #5185, #1516, #7534, #11837, #12520, #754 ) ) ;
#3824 = ADVANCED_FACE ( 'NONE', ( #4356 ), #3383, .F. ) ;
#3825 = VERTEX_POINT ( 'NONE', #5515 ) ;
#3826 = ORIENTED_EDGE ( 'NONE', *, *, #5654, .T. ) ;
#3827 = CARTESIAN_POINT ( 'NONE',  ( 17.00000000000000355, 3.000000000000000000, -14.92471123914605435 ) ) ;
#3828 = VECTOR ( 'NONE', #1372, 1000.000000000000000 ) ;
#3829 = CARTESIAN_POINT ( 'NONE',  ( 7.494008246337245716, 0.000000000000000000, -11.63517940784380578 ) ) ;
#3830 = DIRECTION ( 'NONE',  ( -0.000000000000000000, -0.000000000000000000, 1.000000000000000000 ) ) ;
#3831 = FACE_BOUND ( 'NONE', #6077, .T. ) ;
#3832 = CARTESIAN_POINT ( 'NONE',  ( -2.631756770590896632, 3.000000000000000000, -14.20034848914872505 ) ) ;
#3833 = CARTESIAN_POINT ( 'NONE',  ( 10.69794375946289655, 0.000000000000000000, 7.065816209474157006 ) ) ;
#3834 = DIRECTION ( 'NONE',  ( -0.000000000000000000, -1.000000000000000000, -0.000000000000000000 ) ) ;
#3835 = CIRCLE ( 'NONE', #981, 1.500000000000000666 ) ;
#3836 = CARTESIAN_POINT ( 'NONE',  ( 20.00000000000000355, 0.000000000000000000, -14.92471123914604370 ) ) ;
#3837 = CIRCLE ( 'NONE', #11097, 8.499999999999998224 ) ;
#3838 = ORIENTED_EDGE ( 'NONE', *, *, #607, .F. ) ;
#3839 = ADVANCED_FACE ( 'NONE', ( #11798 ), #1394, .T. ) ;
#3840 = ORIENTED_EDGE ( 'NONE', *, *, #5536, .F. ) ;
#3841 = ORIENTED_EDGE ( 'NONE', *, *, #4998, .T. ) ;
#3842 = DIRECTION ( 'NONE',  ( 0.000000000000000000, 0.000000000000000000, 1.000000000000000000 ) ) ;
#3843 = EDGE_LOOP ( 'NONE', ( #6191, #414, #12556, #2902 ) ) ;
#3844 = EDGE_CURVE ( 'NONE', #1008, #1968, #11860, .T. ) ;
#3845 = CARTESIAN_POINT ( 'NONE',  ( -2.428572470324203980, 0.000000000000000000, -13.33579367773357482 ) ) ;
#3846 = CARTESIAN_POINT ( 'NONE',  ( 5.727824870044268657, 32.33135765298362685, -11.34110233529635359 ) ) ;
#3847 = CIRCLE ( 'NONE', #9349, 14.24999999999999822 ) ;
#3848 = LINE ( 'NONE', #8048, #41 ) ;
#3849 = DIRECTION ( 'NONE',  ( 0.9288742131985401329, 0.000000000000000000, -0.3703953240185316464 ) ) ;
#3850 = CARTESIAN_POINT ( 'NONE',  ( 1.959434878635765477E-16, 0.09999999999999982514, -1.600000000000000311 ) ) ;
#3851 = CARTESIAN_POINT ( 'NONE',  ( 3.542895259386137585, 3.000000000000000000, -12.51336047125611017 ) ) ;
#3852 = FACE_OUTER_BOUND ( 'NONE', #6929, .T. ) ;
#3853 = VERTEX_POINT ( 'NONE', #11657 ) ;
#3854 = ORIENTED_EDGE ( 'NONE', *, *, #7592, .F. ) ;
#3855 = ORIENTED_EDGE ( 'NONE', *, *, #624, .F. ) ;
#3856 = CIRCLE ( 'NONE', #345, 0.1000000000000000472 ) ;
#3857 = CARTESIAN_POINT ( 'NONE',  ( 48.06174015963858892, 0.000000000000000000, -3.086958956539055166 ) ) ;
#3858 = ORIENTED_EDGE ( 'NONE', *, *, #8687, .T. ) ;
#3859 = ORIENTED_EDGE ( 'NONE', *, *, #6600, .F. ) ;
#3860 = FACE_OUTER_BOUND ( 'NONE', #363, .T. ) ;
#3861 = CARTESIAN_POINT ( 'NONE',  ( -13.73660796332618261, 0.000000000000000000, -6.025412986832017204 ) ) ;
#3862 = DIRECTION ( 'NONE',  ( -0.000000000000000000, -1.000000000000000000, -0.000000000000000000 ) ) ;
#3863 = AXIS2_PLACEMENT_3D ( 'NONE', #616, #9209, #4872 ) ;
#3864 = CARTESIAN_POINT ( 'NONE',  ( -14.16466328168009881, 3.000000000000000000, 1.557181465540760534 ) ) ;
#3865 = CARTESIAN_POINT ( 'NONE',  ( 46.02418392430381999, 3.000000000000000000, -15.41988256844266658 ) ) ;
#3866 = DIRECTION ( 'NONE',  ( -0.000000000000000000, -0.000000000000000000, -1.000000000000000000 ) ) ;
#3867 = EDGE_CURVE ( 'NONE', #3324, #7144, #9718, .T. ) ;
#3868 = ORIENTED_EDGE ( 'NONE', *, *, #9266, .T. ) ;
#3869 = DIRECTION ( 'NONE',  ( 0.000000000000000000, 0.000000000000000000, 1.000000000000000000 ) ) ;
#3870 = VERTEX_POINT ( 'NONE', #1255 ) ;
#3871 = ORIENTED_EDGE ( 'NONE', *, *, #1124, .F. ) ;
#3872 = LINE ( 'NONE', #8077, #3130 ) ;
#3873 = B_SPLINE_SURFACE_WITH_KNOTS ( 'NONE', 2, 1, ( 
 ( #10856, #2179 ),
 ( #11886, #4446 ),
 ( #7553, #5415 ) ),
 .UNSPECIFIED., .F., .F., .F.,
 ( 3, 3 ),
 ( 2, 2 ),
 ( 0.000000000000000000, 1.000000000000000000 ),
 ( 0.000000000000000000, 1.000000000000000000 ),
 .UNSPECIFIED. ) ;
#3874 = ORIENTED_EDGE ( 'NONE', *, *, #224, .T. ) ;
#3875 = DIRECTION ( 'NONE',  ( -0.000000000000000000, -1.000000000000000000, -0.000000000000000000 ) ) ;
#3876 = DIRECTION ( 'NONE',  ( 0.000000000000000000, 0.000000000000000000, -1.000000000000000000 ) ) ;
#3877 = CARTESIAN_POINT ( 'NONE',  ( 31.00000000000000000, 3.000000000000000000, 0.000000000000000000 ) ) ;
#3878 = DIRECTION ( 'NONE',  ( 0.000000000000000000, 1.000000000000000000, 0.000000000000000000 ) ) ;
#3879 = CARTESIAN_POINT ( 'NONE',  ( -6.329356821613726147, 3.000000000000000000, -12.30759122142001338 ) ) ;
#3880 = CARTESIAN_POINT ( 'NONE',  ( 10.00000000000000533, 2.749999999999997335, 10.00000000000000178 ) ) ;
#3881 = LINE ( 'NONE', #10979, #13456 ) ;
#3882 = CARTESIAN_POINT ( 'NONE',  ( 4.163799117101002038E-16, 2.900000000000000355, -3.400000000000001243 ) ) ;
#3883 = CARTESIAN_POINT ( 'NONE',  ( 3.818534268238711782, 9.000000000000000000, -5.566084444408534004 ) ) ;
#3884 = EDGE_LOOP ( 'NONE', ( #3470, #13020, #5382, #13016 ) ) ;
#3885 = EDGE_CURVE ( 'NONE', #12227, #11094, #5394, .T. ) ;
#3886 = EDGE_LOOP ( 'NONE', ( #1834, #8435, #4979, #13296 ) ) ;
#3887 = EDGE_CURVE ( 'NONE', #746, #7144, #10570, .T. ) ;
#3888 = ORIENTED_EDGE ( 'NONE', *, *, #11545, .F. ) ;
#3889 = ORIENTED_EDGE ( 'NONE', *, *, #5409, .T. ) ;
#3890 = CARTESIAN_POINT ( 'NONE',  ( 7.499999999999999112, 3.000000000000000000, 0.000000000000000000 ) ) ;
#3891 = LINE ( 'NONE', #8296, #7360 ) ;
#3892 = CARTESIAN_POINT ( 'NONE',  ( -14.90895795148409420, 0.000000000000000000, 1.650143266773909101 ) ) ;
#3893 = EDGE_CURVE ( 'NONE', #6080, #13469, #13207, .T. ) ;
#3894 = DIRECTION ( 'NONE',  ( 0.000000000000000000, -0.000000000000000000, -1.000000000000000000 ) ) ;
#3895 = CARTESIAN_POINT ( 'NONE',  ( 9.573149624528804580, 3.000000000000000000, -8.795158114916638681 ) ) ;
#3896 = CARTESIAN_POINT ( 'NONE',  ( 0.000000000000000000, 14.00000000000000178, 0.000000000000000000 ) ) ;
#3897 = DIRECTION ( 'NONE',  ( -0.000000000000000000, -1.000000000000000000, -0.000000000000000000 ) ) ;
#3898 = ORIENTED_EDGE ( 'NONE', *, *, #866, .F. ) ;
#3899 = EDGE_CURVE ( 'NONE', #291, #9987, #33, .T. ) ;
#3900 = B_SPLINE_SURFACE_WITH_KNOTS ( 'NONE', 3, 1, ( 
 ( #4781, #719 ),
 ( #10078, #8968 ),
 ( #6582, #9115 ),
 ( #13179, #6840 ) ),
 .UNSPECIFIED., .F., .F., .F.,
 ( 4, 4 ),
 ( 2, 2 ),
 ( 0.000000000000000000, 0.8452273900860258760 ),
 ( 0.000000000000000000, 1.000000000000000000 ),
 .UNSPECIFIED. ) ;
#3901 = CARTESIAN_POINT ( 'NONE',  ( 19.60942157306000766, 3.000000000000000000, 14.05941790610251374 ) ) ;
#3902 = CARTESIAN_POINT ( 'NONE',  ( -0.5501230721523990841, 3.000000000000000000, -12.98835496148299384 ) ) ;
#3903 = ORIENTED_EDGE ( 'NONE', *, *, #7030, .T. ) ;
#3904 = CARTESIAN_POINT ( 'NONE',  ( 7.499999999999999112, 0.000000000000000000, 0.000000000000000000 ) ) ;
#3905 = CARTESIAN_POINT ( 'NONE',  ( 5.727824870045131966, 41.33135765298363395, -11.34110233529591483 ) ) ;
#3906 = EDGE_CURVE ( 'NONE', #11282, #4803, #2154, .T. ) ;
#3907 = FACE_OUTER_BOUND ( 'NONE', #8653, .T. ) ;
#3908 = CARTESIAN_POINT ( 'NONE',  ( -5.976238463952679325, 9.000000000000000000, -3.138004751744734477 ) ) ;
#3909 = EDGE_CURVE ( 'NONE', #5272, #2212, #12357, .T. ) ;
#3910 = CARTESIAN_POINT ( 'NONE',  ( 31.00000000000000000, -8.809142651444723526E-17, -1.600000000000004086 ) ) ;
#3911 = MANIFOLD_SOLID_BREP ( 'Fillet1', #5975 ) ;
#3912 = DIRECTION ( 'NONE',  ( -0.000000000000000000, -1.000000000000000000, -0.000000000000000000 ) ) ;
#3913 = CARTESIAN_POINT ( 'NONE',  ( -10.97318381393799136, 0.000000000000000000, -6.970598036433411693 ) ) ;
#3914 = ORIENTED_EDGE ( 'NONE', *, *, #11390, .T. ) ;
#3915 = CARTESIAN_POINT ( 'NONE',  ( 12.48034623170854474, 0.000000000000000000, 4.337627373772809491 ) ) ;
#3916 = VERTEX_POINT ( 'NONE', #11102 ) ;
#3917 = PRODUCT_DEFINITION_CONTEXT ( 'detailed design', #2741, 'design' ) ;
#3918 = VERTEX_POINT ( 'NONE', #12072 ) ;
#3919 = LINE ( 'NONE', #1665, #5113 ) ;
#3920 = ORIENTED_EDGE ( 'NONE', *, *, #2613, .F. ) ;
#3921 = ADVANCED_BREP_SHAPE_REPRESENTATION ( '', ( #13227, #10007 ), #1673 ) ;
#3922 = ORIENTED_EDGE ( 'NONE', *, *, #12261, .T. ) ;
#3923 = CARTESIAN_POINT ( 'NONE',  ( 3.007863545083557355, 9.000000000000000000, 7.350755164602351677 ) ) ;
#3924 = CARTESIAN_POINT ( 'NONE',  ( -5.299649803506881085, 0.000000000000000000, -6.645578376649351249 ) ) ;
#3925 = DIRECTION ( 'NONE',  ( -4.625929269271486900E-15, -1.000000000000000000, 0.000000000000000000 ) ) ;
#3926 = CARTESIAN_POINT ( 'NONE',  ( -8.795158114916672432, 3.000000000000000000, -9.573149624528774382 ) ) ;
#3927 = CARTESIAN_POINT ( 'NONE',  ( 0.000000000000000000, 9.000000000000000000, 0.000000000000000000 ) ) ;
#3928 = FACE_BOUND ( 'NONE', #9012, .T. ) ;
#3929 = EDGE_LOOP ( 'NONE', ( #1047, #5271, #10475, #4064 ) ) ;
#3930 = CARTESIAN_POINT ( 'NONE',  ( -2.655466033450426533, 0.000000000000000000, -7.485541762018160128 ) ) ;
#3931 = ORIENTED_EDGE ( 'NONE', *, *, #13097, .T. ) ;
#3932 = VERTEX_POINT ( 'NONE', #7458 ) ;
#3933 = CARTESIAN_POINT ( 'NONE',  ( 54.70014691233865989, 0.000000000000000000, -3.785783530882224746 ) ) ;
#3934 = CIRCLE ( 'NONE', #3056, 1.499999999999999556 ) ;
#3935 = ORIENTED_EDGE ( 'NONE', *, *, #7589, .T. ) ;
#3936 = ADVANCED_FACE ( 'NONE', ( #5792 ), #9852, .F. ) ;
#3937 = DIRECTION ( 'NONE',  ( 0.000000000000000000, 1.000000000000000000, 0.000000000000000000 ) ) ;
#3938 = CARTESIAN_POINT ( 'NONE',  ( 11.11702303352191912, 3.000000000000000000, -8.914835885878277466 ) ) ;
#3939 = CARTESIAN_POINT ( 'NONE',  ( 0.000000000000000000, 3.000000000000000000, 0.000000000000000000 ) ) ;
#3940 = FACE_OUTER_BOUND ( 'NONE', #6664, .T. ) ;
#3941 = CIRCLE ( 'NONE', #7258, 12.08999999999737440 ) ;
#3942 = DIRECTION ( 'NONE',  ( 0.000000000000000000, 0.000000000000000000, 1.000000000000000000 ) ) ;
#3943 = CARTESIAN_POINT ( 'NONE',  ( 31.00000000000000000, 2.900000000000000355, 0.000000000000000000 ) ) ;
#3944 = CARTESIAN_POINT ( 'NONE',  ( -1.133238802859761973, 3.000000000000000000, -14.39763212228013067 ) ) ;
#3945 = CARTESIAN_POINT ( 'NONE',  ( 11.63517940784358196, 3.000000000000000000, -7.494008246337187096 ) ) ;
#3946 = DIRECTION ( 'NONE',  ( -1.000000000000000000, 0.000000000000000000, -0.000000000000000000 ) ) ;
#3947 = DIRECTION ( 'NONE',  ( -0.000000000000000000, -1.000000000000000000, -0.000000000000000000 ) ) ;
#3948 = VERTEX_POINT ( 'NONE', #13028 ) ;
#3949 = ORIENTED_EDGE ( 'NONE', *, *, #4060, .T. ) ;
#3950 = AXIS2_PLACEMENT_3D ( 'NONE', #12301, #4088, #12510 ) ;
#3951 = ORIENTED_EDGE ( 'NONE', *, *, #141, .F. ) ;
#3952 = EDGE_CURVE ( 'NONE', #10761, #10809, #8331, .T. ) ;
#3953 = EDGE_CURVE ( 'NONE', #76, #11033, #10959, .T. ) ;
#3954 = ORIENTED_EDGE ( 'NONE', *, *, #3274, .F. ) ;
#3955 = CARTESIAN_POINT ( 'NONE',  ( 7.500000000000003553, 0.000000000000000000, 13.39999999999999858 ) ) ;
#3956 = EDGE_CURVE ( 'NONE', #10361, #1111, #11449, .T. ) ;
#3957 = DIRECTION ( 'NONE',  ( -1.000000000000000000, 0.000000000000000000, 0.000000000000000000 ) ) ;
#3958 = CARTESIAN_POINT ( 'NONE',  ( -14.82803603298498629, 3.000000000000000000, 2.264806262023049577 ) ) ;
#3959 = ADVANCED_FACE ( 'NONE', ( #7721 ), #7107, .F. ) ;
#3960 = VECTOR ( 'NONE', #12233, 1000.000000000000000 ) ;
#3961 = DIRECTION ( 'NONE',  ( 0.000000000000000000, 1.000000000000000000, 0.000000000000000000 ) ) ;
#3962 = CARTESIAN_POINT ( 'NONE',  ( -2.830255545554292151, 0.000000000000000000, -12.68816982652971959 ) ) ;
#3963 = VECTOR ( 'NONE', #85, 1000.000000000000000 ) ;
#3964 = DIRECTION ( 'NONE',  ( -0.000000000000000000, -1.000000000000000000, -0.000000000000000000 ) ) ;
#3965 = CARTESIAN_POINT ( 'NONE',  ( 31.00000000000000000, 2.900000000000000355, -3.499999999999999556 ) ) ;
#3966 = ORIENTED_EDGE ( 'NONE', *, *, #9788, .T. ) ;
#3967 = DIRECTION ( 'NONE',  ( 0.000000000000000000, 1.000000000000000000, -0.000000000000000000 ) ) ;
#3968 = CARTESIAN_POINT ( 'NONE',  ( 12.25836857253663581, 0.000000000000000000, 5.784789447945493990 ) ) ;
#3969 = AXIS2_PLACEMENT_3D ( 'NONE', #8511, #5219, #5282 ) ;
#3970 = EDGE_CURVE ( 'NONE', #8320, #13244, #8793, .T. ) ;
#3971 = AXIS2_PLACEMENT_3D ( 'NONE', #11570, #9560, #5477 ) ;
#3972 = ORIENTED_EDGE ( 'NONE', *, *, #8368, .F. ) ;
#3973 = DIRECTION ( 'NONE',  ( 0.000000000000000000, 1.000000000000000000, 0.000000000000000000 ) ) ;
#3974 = EDGE_CURVE ( 'NONE', #1409, #732, #10896, .T. ) ;
#3975 = DIRECTION ( 'NONE',  ( -1.000000000000000000, 0.000000000000000000, -2.891205793294677833E-16 ) ) ;
#3976 = ADVANCED_FACE ( 'NONE', ( #7996 ), #10401, .F. ) ;
#3977 = FACE_OUTER_BOUND ( 'NONE', #3709, .T. ) ;
#3978 = CARTESIAN_POINT ( 'NONE',  ( -5.039625798601655937, 9.000000000000000000, 4.490509081392511703 ) ) ;
#3979 = CARTESIAN_POINT ( 'NONE',  ( -11.11702303352191734, 0.000000000000000000, 8.914835885878279242 ) ) ;
#3980 = AXIS2_PLACEMENT_3D ( 'NONE', #54, #8234, #2938 ) ;
#3981 = CARTESIAN_POINT ( 'NONE',  ( 3.542895259386137585, 0.000000000000000000, -12.51336047125611017 ) ) ;
#3982 = B_SPLINE_SURFACE_WITH_KNOTS ( 'NONE', 3, 1, ( 
 ( #3507, #419 ),
 ( #10819, #8804 ),
 ( #7718, #5651 ),
 ( #1388, #9915 ) ),
 .UNSPECIFIED., .F., .F., .F.,
 ( 4, 4 ),
 ( 2, 2 ),
 ( 0.000000000000000000, 0.5855695330273008592 ),
 ( 0.000000000000000000, 1.000000000000000000 ),
 .UNSPECIFIED. ) ;
#3983 = CIRCLE ( 'NONE', #6188, 1.500000000000000222 ) ;
#3984 = CARTESIAN_POINT ( 'NONE',  ( 2.999999999999995559, 2.000000000000000000, -10.00000000000000355 ) ) ;
#3985 = CARTESIAN_POINT ( 'NONE',  ( -10.34346111134701118, 3.000000000000000000, -8.760376775873707444 ) ) ;
#3986 = VERTEX_POINT ( 'NONE', #12961 ) ;
#3987 = EDGE_LOOP ( 'NONE', ( #11228, #3641, #5133, #6699 ) ) ;
#3988 = DIRECTION ( 'NONE',  ( -0.000000000000000000, -1.000000000000000000, -0.000000000000000000 ) ) ;
#3989 = ADVANCED_FACE ( 'NONE', ( #11931 ), #13558, .T. ) ;
#3990 = VERTEX_POINT ( 'NONE', #12494 ) ;
#3991 = CIRCLE ( 'NONE', #11480, 1.500000000000000222 ) ;
#3992 = CARTESIAN_POINT ( 'NONE',  ( -10.18987059060247624, 0.000000000000000000, -6.506507307819711095 ) ) ;
#3993 = CARTESIAN_POINT ( 'NONE',  ( -7.065816209474154341, 0.000000000000000000, 10.69794375946289833 ) ) ;
#3994 = SURFACE_STYLE_USAGE ( .BOTH. , #12550 ) ;
#3995 = FACE_OUTER_BOUND ( 'NONE', #4775, .T. ) ;
#3996 = LINE ( 'NONE', #2900, #2457 ) ;
#3997 = CARTESIAN_POINT ( 'NONE',  ( 1.650143266773734796, 0.000000000000000000, -14.90895795148410841 ) ) ;
#3998 = ORIENTED_EDGE ( 'NONE', *, *, #5571, .F. ) ;
#3999 = AXIS2_PLACEMENT_3D ( 'NONE', #2382, #6578, #6517 ) ;
#4000 = CARTESIAN_POINT ( 'NONE',  ( 10.18979803820051622, 3.000000000000000000, -6.506620931068703761 ) ) ;
#4001 = AXIS2_PLACEMENT_3D ( 'NONE', #13216, #12056, #7978 ) ;
#4002 = ORIENTED_EDGE ( 'NONE', *, *, #9779, .F. ) ;
#4003 = ORIENTED_EDGE ( 'NONE', *, *, #3953, .T. ) ;
#4004 = CARTESIAN_POINT ( 'NONE',  ( -2.481593227817846525, 9.000000000000000000, -8.129679886173168057 ) ) ;
#4005 = MANIFOLD_SOLID_BREP ( 'Boss-Extrude1', #4212 ) ;
#4006 = ADVANCED_FACE ( 'NONE', ( #12430 ), #10128, .T. ) ;
#4007 = EDGE_CURVE ( 'NONE', #11354, #12771, #701, .T. ) ;
#4008 = ORIENTED_EDGE ( 'NONE', *, *, #12061, .T. ) ;
#4009 = B_SPLINE_CURVE_WITH_KNOTS ( 'NONE', 3,
 ( #3040, #10554, #11652, #7251 ),
 .UNSPECIFIED., .F., .F.,
 ( 4, 4 ),
 ( 0.1276832474596231171, 1.000000000000000000 ),
 .UNSPECIFIED. ) ;
#4010 = CARTESIAN_POINT ( 'NONE',  ( -14.90895795148409420, 0.000000000000000000, 1.650143266773909101 ) ) ;
#4011 = CIRCLE ( 'NONE', #6653, 12.99999999999977973 ) ;
#4012 = CARTESIAN_POINT ( 'NONE',  ( 10.18979803820051622, 3.000000000000000000, -6.506620931068703761 ) ) ;
#4013 = AXIS2_PLACEMENT_3D ( 'NONE', #8605, #10558, #1119 ) ;
#4014 = CIRCLE ( 'NONE', #4449, 12.08999999999737263 ) ;
#4015 = CARTESIAN_POINT ( 'NONE',  ( 11.70905276178455878, 0.000000000000000000, -9.375397774054460953 ) ) ;
#4016 = DIRECTION ( 'NONE',  ( 0.000000000000000000, 0.000000000000000000, 1.000000000000000000 ) ) ;
#4017 = DIRECTION ( 'NONE',  ( 0.000000000000000000, 1.000000000000000000, -0.000000000000000000 ) ) ;
#4018 = CARTESIAN_POINT ( 'NONE',  ( -7.780961115628988622, 0.000000000000000000, -3.421497350147985728 ) ) ;
#4019 = B_SPLINE_SURFACE_WITH_KNOTS ( 'NONE', 3, 1, ( 
 ( #8729, #8862 ),
 ( #11844, #2403 ),
 ( #4808, #8935 ),
 ( #3695, #7897 ) ),
 .UNSPECIFIED., .F., .F., .F.,
 ( 4, 4 ),
 ( 2, 2 ),
 ( 0.1276832474596231171, 1.000000000000000000 ),
 ( 0.000000000000000000, 1.000000000000000000 ),
 .UNSPECIFIED. ) ;
#4020 = LINE ( 'NONE', #4092, #1103 ) ;
#4021 = DIRECTION ( 'NONE',  ( -0.000000000000000000, -1.000000000000000000, -0.000000000000000000 ) ) ;
#4022 = B_SPLINE_CURVE_WITH_KNOTS ( 'NONE', 3,
 ( #4041, #6110, #1774, #8105 ),
 .UNSPECIFIED., .F., .F.,
 ( 4, 4 ),
 ( 0.000000000000000000, 0.8452273900860258760 ),
 .UNSPECIFIED. ) ;
#4023 = ORIENTED_EDGE ( 'NONE', *, *, #8102, .F. ) ;
#4024 = CARTESIAN_POINT ( 'NONE',  ( 5.170206418547656391, 0.000000000000000000, 13.27898586450067064 ) ) ;
#4025 = ORIENTED_EDGE ( 'NONE', *, *, #8257, .F. ) ;
#4026 = AXIS2_PLACEMENT_3D ( 'NONE', #8261, #12739, #12880 ) ;
#4027 = ORIENTED_EDGE ( 'NONE', *, *, #5513, .T. ) ;
#4028 = AXIS2_PLACEMENT_3D ( 'NONE', #2970, #1037, #7035 ) ;
#4029 = ORIENTED_EDGE ( 'NONE', *, *, #7416, .F. ) ;
#4030 = ORIENTED_EDGE ( 'NONE', *, *, #8822, .F. ) ;
#4031 = CARTESIAN_POINT ( 'NONE',  ( -7.780961115628980629, 0.000000000000000000, -3.421497350147988392 ) ) ;
#4032 = FILL_AREA_STYLE ('',( #10444 ) ) ;
#4033 = VECTOR ( 'NONE', #526, 1000.000000000000000 ) ;
#4034 = CARTESIAN_POINT ( 'NONE',  ( -5.039625798601655937, 9.000000000000000000, 4.490509081392509927 ) ) ;
#4035 = CIRCLE ( 'NONE', #8429, 1.500000000000003997 ) ;
#4036 = AXIS2_PLACEMENT_3D ( 'NONE', #1793, #1930, #5987 ) ;
#4037 = CARTESIAN_POINT ( 'NONE',  ( 7.500000000000003553, 0.000000000000000000, 4.899999999999997691 ) ) ;
#4038 = CARTESIAN_POINT ( 'NONE',  ( -12.30759122141990325, 3.000000000000000000, -6.329356821613475681 ) ) ;
#4039 = DIRECTION ( 'NONE',  ( 0.000000000000000000, 0.000000000000000000, 1.000000000000000000 ) ) ;
#4040 = ADVANCED_FACE ( 'NONE', ( #13378 ), #10272, .F. ) ;
#4041 = CARTESIAN_POINT ( 'NONE',  ( 13.04554897075798081, 3.000000000000000000, -5.733772933379503556 ) ) ;
#4042 = VERTEX_POINT ( 'NONE', #974 ) ;
#4043 = CARTESIAN_POINT ( 'NONE',  ( 7.940744365623959133, 0.000000000000000000, 0.1715058177969961128 ) ) ;
#4044 = AXIS2_PLACEMENT_3D ( 'NONE', #13404, #7212, #3062 ) ;
#4045 = DIRECTION ( 'NONE',  ( 0.000000000000000000, 0.000000000000000000, -1.000000000000000000 ) ) ;
#4046 = EDGE_LOOP ( 'NONE', ( #10240, #6959, #10748, #4615 ) ) ;
#4047 = CARTESIAN_POINT ( 'NONE',  ( 0.000000000000000000, 0.000000000000000000, -1.500000000000000222 ) ) ;
#4048 = APPLICATION_PROTOCOL_DEFINITION ( 'draft international standard', 'automotive_design', 1998, #7231 ) ;
#4049 = CARTESIAN_POINT ( 'NONE',  ( 1.119409668803368119, 3.000000000000000000, 13.50845331674225847 ) ) ;
#4050 = CARTESIAN_POINT ( 'NONE',  ( 4.056222772158357692, 0.000000000000000000, -12.16218796965919680 ) ) ;
#4051 = AXIS2_PLACEMENT_3D ( 'NONE', #12470, #7216, #6172 ) ;
#4052 = DIRECTION ( 'NONE',  ( -1.927470528863118802E-16, 0.000000000000000000, 1.000000000000000000 ) ) ;
#4053 = AXIS2_PLACEMENT_3D ( 'NONE', #12272, #2811, #4605 ) ;
#4054 = ADVANCED_FACE ( 'NONE', ( #10332 ), #12399, .T. ) ;
#4055 = CARTESIAN_POINT ( 'NONE',  ( -7.125870497355421662, 0.000000000000000000, -3.507536778237742237 ) ) ;
#4056 = EDGE_CURVE ( 'NONE', #7832, #6591, #13576, .T. ) ;
#4057 = CARTESIAN_POINT ( 'NONE',  ( 29.02231267299996986, 3.000000000000000000, -1.321950885510182250 ) ) ;
#4058 = VERTEX_POINT ( 'NONE', #8069 ) ;
#4059 = UNCERTAINTY_MEASURE_WITH_UNIT (LENGTH_MEASURE( 1.000000000000000082E-05 ), #5864, 'distance_accuracy_value', 'NONE');
#4060 = EDGE_CURVE ( 'NONE', #4189, #9400, #12115, .T. ) ;
#4061 = VERTEX_POINT ( 'NONE', #7241 ) ;
#4062 = DIRECTION ( 'NONE',  ( 0.000000000000000000, 0.000000000000000000, -1.000000000000000000 ) ) ;
#4063 = ADVANCED_FACE ( 'NONE', ( #2828 ), #4070, .T. ) ;
#4064 = ORIENTED_EDGE ( 'NONE', *, *, #2232, .T. ) ;
#4065 = COLOUR_RGB ( '',0.7803921568627451011, 0.7607843137254901578, 0.7411764705882353255 ) ;
#4066 = AXIS2_PLACEMENT_3D ( 'NONE', #1469, #3317, #4423 ) ;
#4067 = CIRCLE ( 'NONE', #13539, 0.4000000000000000222 ) ;
#4068 = CARTESIAN_POINT ( 'NONE',  ( 2.620242232815953809, 0.000000000000000000, 6.881105251569436199 ) ) ;
#4069 = CARTESIAN_POINT ( 'NONE',  ( 12.00000000000001599, 6.750000000000000000, -2.770445225425678373E-15 ) ) ;
#4070 = CYLINDRICAL_SURFACE ( 'NONE', #12344, 2.500000000000000444 ) ;
#4071 = DIRECTION ( 'NONE',  ( 0.000000000000000000, 1.000000000000000000, -0.000000000000000000 ) ) ;
#4072 = EDGE_CURVE ( 'NONE', #13228, #10250, #1116, .T. ) ;
#4073 = DIRECTION ( 'NONE',  ( -0.000000000000000000, -1.000000000000000000, -0.000000000000000000 ) ) ;
#4074 = CARTESIAN_POINT ( 'NONE',  ( -10.72979803820132183, 0.000000000000000000, -5.571313494980132397 ) ) ;
#4075 = ORIENTED_EDGE ( 'NONE', *, *, #10649, .T. ) ;
#4076 =( GEOMETRIC_REPRESENTATION_CONTEXT ( 3 ) GLOBAL_UNCERTAINTY_ASSIGNED_CONTEXT ( ( #10811 ) ) GLOBAL_UNIT_ASSIGNED_CONTEXT ( ( #11858, #1390, #6555 ) ) REPRESENTATION_CONTEXT ( 'NONE', 'WORKASPACE' ) );
#4077 = CARTESIAN_POINT ( 'NONE',  ( 0.000000000000000000, 0.000000000000000000, 0.000000000000000000 ) ) ;
#4078 = AXIS2_PLACEMENT_3D ( 'NONE', #8717, #3273, #2186 ) ;
#4079 = EDGE_LOOP ( 'NONE', ( #7404, #2460 ) ) ;
#4080 = EDGE_LOOP ( 'NONE', ( #12049, #4926, #1107, #10377 ) ) ;
#4081 = CARTESIAN_POINT ( 'NONE',  ( -8.158651161643904359, 0.000000000000000000, -8.922136023539605887 ) ) ;
#4082 = ADVANCED_FACE ( 'NONE', ( #1806 ), #6001, .F. ) ;
#4083 = VERTEX_POINT ( 'NONE', #12811 ) ;
#4084 = PLANE ( 'NONE',  #8441 ) ;
#4085 = PRESENTATION_LAYER_ASSIGNMENT (  '', '', ( #12243 ) ) ;
#4086 = CARTESIAN_POINT ( 'NONE',  ( 6.000000000000008882, 3.000000000000000000, 25.50000000000000000 ) ) ;
#4087 = CARTESIAN_POINT ( 'NONE',  ( -0.5501230721523990841, 3.000000000000000000, -12.98835496148299384 ) ) ;
#4088 = DIRECTION ( 'NONE',  ( -0.000000000000000000, -1.000000000000000000, -0.000000000000000000 ) ) ;
#4089 = FACE_OUTER_BOUND ( 'NONE', #6208, .T. ) ;
#4090 = CARTESIAN_POINT ( 'NONE',  ( 0.000000000000000000, 0.000000000000000000, 0.000000000000000000 ) ) ;
#4091 = EDGE_CURVE ( 'NONE', #7238, #3870, #4851, .T. ) ;
#4092 = CARTESIAN_POINT ( 'NONE',  ( -5.170206418547658167, 3.000000000000000000, -13.27898586450066887 ) ) ;
#4093 = LINE ( 'NONE', #2923, #7517 ) ;
#4094 = DIRECTION ( 'NONE',  ( 0.000000000000000000, 0.000000000000000000, -1.000000000000000000 ) ) ;
#4095 = ORIENTED_EDGE ( 'NONE', *, *, #11148, .T. ) ;
#4096 = DIRECTION ( 'NONE',  ( -0.000000000000000000, -1.000000000000000000, -0.000000000000000000 ) ) ;
#4097 = VERTEX_POINT ( 'NONE', #3230 ) ;
#4098 = AXIS2_PLACEMENT_3D ( 'NONE', #3767, #822, #2808 ) ;
#4099 = ORIENTED_EDGE ( 'NONE', *, *, #5220, .T. ) ;
#4100 = EDGE_CURVE ( 'NONE', #3538, #9570, #1300, .T. ) ;
#4101 = ORIENTED_EDGE ( 'NONE', *, *, #6279, .T. ) ;
#4102 = ORIENTED_EDGE ( 'NONE', *, *, #4007, .T. ) ;
#4103 = DIRECTION ( 'NONE',  ( 0.000000000000000000, 0.000000000000000000, -1.000000000000000000 ) ) ;
#4104 = DIRECTION ( 'NONE',  ( -0.9893737785712105604, -0.000000000000000000, 0.1453943818575021141 ) ) ;
#4105 = CARTESIAN_POINT ( 'NONE',  ( 0.000000000000000000, 0.000000000000000000, 0.000000000000000000 ) ) ;
#4106 = LINE ( 'NONE', #3129, #9476 ) ;
#4107 = CARTESIAN_POINT ( 'NONE',  ( -13.50994833511691340, 3.000000000000000000, -1.105736515254444052 ) ) ;
#4108 = EDGE_LOOP ( 'NONE', ( #13586, #6102, #4548, #10588 ) ) ;
#4109 = ADVANCED_FACE ( 'NONE', ( #1169 ), #8589, .F. ) ;
#4110 = CARTESIAN_POINT ( 'NONE',  ( 30.79170750349150509, 3.000000000000000000, -0.0004760053210284623249 ) ) ;
#4111 = CARTESIAN_POINT ( 'NONE',  ( 30.79170750349150509, 3.000000000000000000, -0.0004760053210284623249 ) ) ;
#4112 = ORIENTED_EDGE ( 'NONE', *, *, #10962, .F. ) ;
#4113 = LINE ( 'NONE', #629, #1623 ) ;
#4114 = ADVANCED_FACE ( 'NONE', ( #3287 ), #6112, .F. ) ;
#4115 = CARTESIAN_POINT ( 'NONE',  ( 48.06174015963858892, 3.000000000000000000, -3.086958956539055166 ) ) ;
#4116 = APPLICATION_PROTOCOL_DEFINITION ( 'draft international standard', 'automotive_design', 1998, #10822 ) ;
#4117 = CARTESIAN_POINT ( 'NONE',  ( -11.52330688609014686, 0.000000000000000000, -6.017756925049552841 ) ) ;
#4118 = LINE ( 'NONE', #3219, #9468 ) ;
#4119 = CARTESIAN_POINT ( 'NONE',  ( 2.264806262022877714, 0.000000000000000000, -14.82803603298501471 ) ) ;
#4120 = CARTESIAN_POINT ( 'NONE',  ( -11.17001009226120445, 3.000000000000000000, -6.660869730750943241 ) ) ;
#4121 = CARTESIAN_POINT ( 'NONE',  ( -9.600126836553261711, 0.000000000000000000, -8.482622935103767858 ) ) ;
#4122 = ORIENTED_EDGE ( 'NONE', *, *, #10783, .F. ) ;
#4123 = ORIENTED_EDGE ( 'NONE', *, *, #11037, .T. ) ;
#4124 = EDGE_LOOP ( 'NONE', ( #658, #3000, #7192, #2586 ) ) ;
#4125 = DIRECTION ( 'NONE',  ( 0.000000000000000000, 1.000000000000000000, -0.000000000000000000 ) ) ;
#4126 = ORIENTED_EDGE ( 'NONE', *, *, #2939, .T. ) ;
#4127 = B_SPLINE_CURVE_WITH_KNOTS ( 'NONE', 3,
 ( #9355, #8443, #4174, #1079 ),
 .UNSPECIFIED., .F., .F.,
 ( 4, 4 ),
 ( 0.1276832474596281686, 1.000000000000000000 ),
 .UNSPECIFIED. ) ;
#4128 = EDGE_CURVE ( 'NONE', #10071, #6484, #7575, .T. ) ;
#4129 = CARTESIAN_POINT ( 'NONE',  ( 8.795158114916441505, 3.000000000000000000, -9.573149624528689117 ) ) ;
#4130 = EDGE_CURVE ( 'NONE', #9203, #5441, #8811, .T. ) ;
#4131 = CARTESIAN_POINT ( 'NONE',  ( 5.733772933379453818, 3.000000000000000000, 13.04554897075800568 ) ) ;
#4132 = CARTESIAN_POINT ( 'NONE',  ( 0.7868956173019259204, 9.000000000000000000, 7.903520140620750034 ) ) ;
#4133 = CARTESIAN_POINT ( 'NONE',  ( -11.70905276178463872, 3.000000000000000000, -9.375397774054366806 ) ) ;
#4134 = EDGE_CURVE ( 'NONE', #1296, #672, #4631, .T. ) ;
#4135 = CARTESIAN_POINT ( 'NONE',  ( 0.8653219153705552502, 0.000000000000000000, -7.312626806738413698 ) ) ;
#4136 = CARTESIAN_POINT ( 'NONE',  ( 22.00000000000000000, 0.000000000000000000, 1.500000000000000666 ) ) ;
#4137 = ORIENTED_EDGE ( 'NONE', *, *, #11384, .F. ) ;
#4138 = CARTESIAN_POINT ( 'NONE',  ( 0.000000000000000000, 0.000000000000000000, 0.000000000000000000 ) ) ;
#4139 = VERTEX_POINT ( 'NONE', #8664 ) ;
#4140 = ORIENTED_EDGE ( 'NONE', *, *, #10526, .T. ) ;
#4141 = DIRECTION ( 'NONE',  ( -0.000000000000000000, -1.000000000000000000, -0.000000000000000000 ) ) ;
#4142 = ORIENTED_EDGE ( 'NONE', *, *, #1447, .T. ) ;
#4143 = APPLICATION_CONTEXT ( 'automotive_design' ) ;
#4144 = EDGE_CURVE ( 'NONE', #11098, #578, #1780, .T. ) ;
#4145 = CYLINDRICAL_SURFACE ( 'NONE', #10002, 6.749999999999999112 ) ;
#4146 = CARTESIAN_POINT ( 'NONE',  ( 6.970598036433451661, 3.000000000000000000, -10.97318381393796294 ) ) ;
#4147 = CARTESIAN_POINT ( 'NONE',  ( 5.280889752749253319, 9.000000000000000000, -6.660495733750448011 ) ) ;
#4148 = CARTESIAN_POINT ( 'NONE',  ( 11.11702303352196708, 0.000000000000000000, 8.914835885878218846 ) ) ;
#4149 = DIRECTION ( 'NONE',  ( 0.7216024245882196597, 0.000000000000000000, -0.6923076923076926237 ) ) ;
#4150 = CARTESIAN_POINT ( 'NONE',  ( -6.549210654805285081, 9.000000000000000000, 1.634117437329677180 ) ) ;
#4151 = ADVANCED_FACE ( 'NONE', ( #10609 ), #2195, .T. ) ;
#4152 = CARTESIAN_POINT ( 'NONE',  ( -4.340891659662447388, 0.000000000000000000, 6.651128039276029469 ) ) ;
#4153 = CARTESIAN_POINT ( 'NONE',  ( -5.976238463952679325, 0.000000000000000000, -3.138004751744733589 ) ) ;
#4154 = ORIENTED_EDGE ( 'NONE', *, *, #6084, .F. ) ;
#4155 = CARTESIAN_POINT ( 'NONE',  ( 7.499999999999999112, 0.000000000000000000, 1.499999999999997780 ) ) ;
#4156 = ORIENTED_EDGE ( 'NONE', *, *, #13079, .F. ) ;
#4157 = ORIENTED_EDGE ( 'NONE', *, *, #12051, .T. ) ;
#4158 = ORIENTED_EDGE ( 'NONE', *, *, #5458, .T. ) ;
#4159 = EDGE_CURVE ( 'NONE', #2677, #12749, #306, .T. ) ;
#4160 = EDGE_CURVE ( 'NONE', #13268, #5502, #6821, .T. ) ;
#4161 = ORIENTED_EDGE ( 'NONE', *, *, #12581, .F. ) ;
#4162 = CARTESIAN_POINT ( 'NONE',  ( -2.830255545554292151, 3.000000000000000000, -12.68816982652971959 ) ) ;
#4163 = CARTESIAN_POINT ( 'NONE',  ( 7.702138240596505092, 0.000000000000000000, -30.99999999999999289 ) ) ;
#4164 = LINE ( 'NONE', #7213, #9079 ) ;
#4165 = CARTESIAN_POINT ( 'NONE',  ( -11.80615107470192804, 0.000000000000000000, -2.604399508764160487 ) ) ;
#4166 = CYLINDRICAL_SURFACE ( 'NONE', #1568, 12.99999999999977973 ) ;
#4167 = CIRCLE ( 'NONE', #1093, 3.100000000000000533 ) ;
#4168 = ORIENTED_EDGE ( 'NONE', *, *, #11566, .F. ) ;
#4169 = ORIENTED_EDGE ( 'NONE', *, *, #5148, .T. ) ;
#4170 = DIRECTION ( 'NONE',  ( 0.000000000000000000, 0.000000000000000000, 1.000000000000000000 ) ) ;
#4171 = CARTESIAN_POINT ( 'NONE',  ( 40.92955321648837241, 0.000000000000000000, -6.070049343411170639 ) ) ;
#4172 = EDGE_CURVE ( 'NONE', #464, #4566, #7379, .T. ) ;
#4173 = EDGE_LOOP ( 'NONE', ( #11072, #8000, #7691, #2410 ) ) ;
#4174 = CARTESIAN_POINT ( 'NONE',  ( -4.190859029938718727, 9.000000000000000000, -6.054087828318142073 ) ) ;
#4175 = CIRCLE ( 'NONE', #2199, 0.1000000000000001166 ) ;
#4176 = VECTOR ( 'NONE', #8282, 1000.000000000000000 ) ;
#4177 = FACE_OUTER_BOUND ( 'NONE', #4608, .T. ) ;
#4178 = CARTESIAN_POINT ( 'NONE',  ( 42.17696780347060326, 31.33135765298363751, 35.00042399990211095 ) ) ;
#4179 = LINE ( 'NONE', #11690, #8803 ) ;
#4180 = FACE_OUTER_BOUND ( 'NONE', #6889, .T. ) ;
#4181 = CARTESIAN_POINT ( 'NONE',  ( 4.898587196589413075E-17, 9.000000000000000000, 0.4000000000000000222 ) ) ;
#4182 = CARTESIAN_POINT ( 'NONE',  ( -14.82803603298502360, 0.000000000000000000, -2.264806262022826644 ) ) ;
#4183 = CYLINDRICAL_SURFACE ( 'NONE', #4258, 1.499999999999997780 ) ;
#4184 = AXIS2_PLACEMENT_3D ( 'NONE', #11330, #4017, #3942 ) ;
#4185 = ORIENTED_EDGE ( 'NONE', *, *, #6647, .T. ) ;
#4186 = VECTOR ( 'NONE', #10479, 1000.000000000000000 ) ;
#4187 = ORIENTED_EDGE ( 'NONE', *, *, #12187, .T. ) ;
#4188 = DIRECTION ( 'NONE',  ( -0.000000000000000000, -1.000000000000000000, -0.000000000000000000 ) ) ;
#4189 = VERTEX_POINT ( 'NONE', #11583 ) ;
#4190 = LINE ( 'NONE', #5229, #221 ) ;
#4191 = FILL_AREA_STYLE_COLOUR ( '', #2540 ) ;
#4192 = CIRCLE ( 'NONE', #2650, 1.500000000000000222 ) ;
#4193 = CARTESIAN_POINT ( 'NONE',  ( -14.20034848914871795, 0.000000000000000000, 2.631756770590945482 ) ) ;
#4194 = CARTESIAN_POINT ( 'NONE',  ( 5.784789447945496654, 3.000000000000000000, -12.25836857253663581 ) ) ;
#4195 = AXIS2_PLACEMENT_3D ( 'NONE', #13012, #7641, #9899 ) ;
#4196 = DIRECTION ( 'NONE',  ( 0.000000000000000000, 0.000000000000000000, -1.000000000000000000 ) ) ;
#4197 = DIRECTION ( 'NONE',  ( 0.000000000000000000, 0.000000000000000000, -1.000000000000000000 ) ) ;
#4198 = CARTESIAN_POINT ( 'NONE',  ( 7.499999999999999112, 3.000000000000000000, 0.000000000000000000 ) ) ;
#4199 = ORIENTED_EDGE ( 'NONE', *, *, #3274, .T. ) ;
#4200 = CARTESIAN_POINT ( 'NONE',  ( -2.411622991978543684, 0.000000000000000000, -6.304488444319686913 ) ) ;
#4201 = VERTEX_POINT ( 'NONE', #2137 ) ;
#4202 = EDGE_CURVE ( 'NONE', #6430, #1110, #11670, .T. ) ;
#4203 = ORIENTED_EDGE ( 'NONE', *, *, #2703, .F. ) ;
#4204 = DIRECTION ( 'NONE',  ( 0.000000000000000000, 0.000000000000000000, -1.000000000000000000 ) ) ;
#4205 = AXIS2_PLACEMENT_3D ( 'NONE', #1831, #10150, #7809 ) ;
#4206 = EDGE_LOOP ( 'NONE', ( #9644, #8816, #4374, #8749, #8121, #13546, #10810, #5937, #4312, #12062, #6715, #4488, #12878, #7693, #11634, #12361 ) ) ;
#4207 = DIRECTION ( 'NONE',  ( 0.000000000000000000, 0.000000000000000000, 1.000000000000000000 ) ) ;
#4208 = DIRECTION ( 'NONE',  ( 1.000000000000000000, 0.000000000000000000, -1.269138026879196405E-16 ) ) ;
#4209 = CARTESIAN_POINT ( 'NONE',  ( 2.601737331980797041, 0.000000000000000000, -6.888123234756056590 ) ) ;
#4210 = CARTESIAN_POINT ( 'NONE',  ( -9.133371500908470608, 0.000000000000000000, -11.90284147956855065 ) ) ;
#4211 = CARTESIAN_POINT ( 'NONE',  ( -2.411622991978541464, 0.000000000000000000, -6.304488444319688689 ) ) ;
#4212 = CLOSED_SHELL ( 'NONE', ( #9843, #12684, #8661, #9142, #12513, #10660, #4820, #2630, #2797, #10505, #700, #3316, #6262, #6772, #1206, #5901, #13575, #7091, #3976, #4624, #8083, #13182, #5086, #8767, #7569, #10700, #12154, #10890, #1221, #5432, #5326, #6181, #10852, #520, #429, #9613, #12923, #9190, #5389, #10924, #5096, #12297, #6506, #11638, #12454, #2722, #11560, #12246, #12495, #7076, #1705, #2646, #567, #2127, #9955, #9755, #1772, #6337, #6740, #12328, #5153, #2039, #8575, #6090 ) ) ;
#4213 = FACE_OUTER_BOUND ( 'NONE', #9232, .T. ) ;
#4214 = VECTOR ( 'NONE', #10335, 1000.000000000000227 ) ;
#4215 = CARTESIAN_POINT ( 'NONE',  ( -12.68816982652970893, 0.000000000000000000, 2.830255545554337004 ) ) ;
#4216 = CARTESIAN_POINT ( 'NONE',  ( -2.428572470324203980, 0.000000000000000000, -13.33579367773357482 ) ) ;
#4217 = EDGE_LOOP ( 'NONE', ( #12111, #7925 ) ) ;
#4218 = FACE_OUTER_BOUND ( 'NONE', #3823, .T. ) ;
#4219 = B_SPLINE_SURFACE_WITH_KNOTS ( 'NONE', 2, 1, ( 
 ( #3272, #10669 ),
 ( #7489, #2330 ),
 ( #9685, #8449 ) ),
 .UNSPECIFIED., .F., .F., .F.,
 ( 3, 3 ),
 ( 2, 2 ),
 ( 0.000000000000000000, 1.000000000000000000 ),
 ( 0.000000000000000000, 1.000000000000000000 ),
 .UNSPECIFIED. ) ;
#4220 = EDGE_CURVE ( 'NONE', #13138, #6731, #11002, .T. ) ;
#4221 = ORIENTED_EDGE ( 'NONE', *, *, #5062, .F. ) ;
#4222 = EDGE_CURVE ( 'NONE', #8880, #6099, #8464, .T. ) ;
#4223 = ORIENTED_EDGE ( 'NONE', *, *, #1134, .F. ) ;
#4224 = ORIENTED_EDGE ( 'NONE', *, *, #4509, .F. ) ;
#4225 = ADVANCED_FACE ( 'NONE', ( #12052 ), #4019, .T. ) ;
#4226 = CIRCLE ( 'NONE', #11933, 0.1000000000000000472 ) ;
#4227 = ADVANCED_FACE ( 'NONE', ( #6602 ), #13217, .T. ) ;
#4228 = CIRCLE ( 'NONE', #11934, 12.08999999999737440 ) ;
#4229 = ORIENTED_EDGE ( 'NONE', *, *, #7893, .T. ) ;
#4230 = CARTESIAN_POINT ( 'NONE',  ( 3.000000000000001776, 0.000000000000000000, 7.000000000000000000 ) ) ;
#4231 = SURFACE_SIDE_STYLE ('',( #242 ) ) ;
#4232 = PLANE ( 'NONE',  #4692 ) ;
#4233 = DIRECTION ( 'NONE',  ( 0.000000000000000000, 1.000000000000000000, 0.000000000000000000 ) ) ;
#4234 = FACE_OUTER_BOUND ( 'NONE', #5627, .T. ) ;
#4235 = AXIS2_PLACEMENT_3D ( 'NONE', #787, #1746, #643 ) ;
#4236 = DIRECTION ( 'NONE',  ( -0.000000000000000000, -1.000000000000000000, -0.000000000000000000 ) ) ;
#4237 = CIRCLE ( 'NONE', #3356, 3.000000000000002665 ) ;
#4238 = AXIS2_PLACEMENT_3D ( 'NONE', #6225, #862, #5053 ) ;
#4239 = ORIENTED_EDGE ( 'NONE', *, *, #10280, .T. ) ;
#4240 = ORIENTED_EDGE ( 'NONE', *, *, #290, .T. ) ;
#4241 = B_SPLINE_SURFACE_WITH_KNOTS ( 'NONE', 3, 1, ( 
 ( #10181, #5015 ),
 ( #13423, #8177 ),
 ( #12480, #12409 ),
 ( #3018, #7225 ) ),
 .UNSPECIFIED., .F., .F., .F.,
 ( 4, 4 ),
 ( 2, 2 ),
 ( 0.1547128134717859205, 1.000000000000000000 ),
 ( 0.000000000000000000, 1.000000000000000000 ),
 .UNSPECIFIED. ) ;
#4242 = DIRECTION ( 'NONE',  ( 0.000000000000000000, 0.000000000000000000, 1.000000000000000000 ) ) ;
#4243 = ORIENTED_EDGE ( 'NONE', *, *, #11709, .F. ) ;
#4244 = CARTESIAN_POINT ( 'NONE',  ( -10.18987059060247624, 3.000000000000000000, -6.506507307819711095 ) ) ;
#4245 = TOROIDAL_SURFACE ( 'NONE', #12177, 3.400000000000001243, 0.1000000000000000056 ) ;
#4246 = PRODUCT_DEFINITION_SHAPE ( 'NONE', 'NONE',  #5460 ) ;
#4247 = AXIS2_PLACEMENT_3D ( 'NONE', #8626, #2436, #3530 ) ;
#4248 = AXIS2_PLACEMENT_3D ( 'NONE', #8669, #355, #1180 ) ;
#4249 = CARTESIAN_POINT ( 'NONE',  ( 0.000000000000000000, 0.000000000000000000, 0.000000000000000000 ) ) ;
#4250 = CARTESIAN_POINT ( 'NONE',  ( 26.30958424017656938, 0.09999999999999982514, 1.500000000000000000 ) ) ;
#4251 = DIRECTION ( 'NONE',  ( 0.000000000000000000, 1.000000000000000000, 0.000000000000000000 ) ) ;
#4252 = LINE ( 'NONE', #4527, #12440 ) ;
#4253 = EDGE_CURVE ( 'NONE', #9985, #11282, #8159, .T. ) ;
#4254 = CARTESIAN_POINT ( 'NONE',  ( 2.928250210355320959, 0.000000000000000000, -13.52637830886121506 ) ) ;
#4255 = VECTOR ( 'NONE', #2849, 1000.000000000000000 ) ;
#4256 = CARTESIAN_POINT ( 'NONE',  ( 4.072642252455978884, 0.000000000000000000, 12.14623037080101042 ) ) ;
#4257 = VECTOR ( 'NONE', #1880, 1000.000000000000000 ) ;
#4258 = AXIS2_PLACEMENT_3D ( 'NONE', #10262, #891, #11298 ) ;
#4259 = ORIENTED_EDGE ( 'NONE', *, *, #10875, .T. ) ;
#4260 = ORIENTED_EDGE ( 'NONE', *, *, #4172, .F. ) ;
#4261 = ORIENTED_EDGE ( 'NONE', *, *, #8879, .F. ) ;
#4262 = CARTESIAN_POINT ( 'NONE',  ( 0.7944557581062196006, 9.000000000000000000, -6.703084368289862205 ) ) ;
#4263 = EDGE_LOOP ( 'NONE', ( #7861, #7877, #13073, #8192, #8962 ) ) ;
#4264 = DIRECTION ( 'NONE',  ( -0.000000000000000000, -1.000000000000000000, 0.000000000000000000 ) ) ;
#4265 = VECTOR ( 'NONE', #3834, 1000.000000000000000 ) ;
#4266 = SURFACE_STYLE_FILL_AREA ( #7304 ) ;
#4267 = AXIS2_PLACEMENT_3D ( 'NONE', #1860, #3081, #10183 ) ;
#4268 = CARTESIAN_POINT ( 'NONE',  ( 6.025412986832064277, 0.000000000000000000, -13.73660796332615597 ) ) ;
#4269 = DIRECTION ( 'NONE',  ( 0.000000000000000000, 1.000000000000000000, 0.000000000000000000 ) ) ;
#4270 = CIRCLE ( 'NONE', #6043, 6.750000000000000888 ) ;
#4271 = CARTESIAN_POINT ( 'NONE',  ( 0.000000000000000000, 0.000000000000000000, 0.000000000000000000 ) ) ;
#4272 = CARTESIAN_POINT ( 'NONE',  ( 2.604531154829233586, 3.000000000000000000, 11.80612203322752585 ) ) ;
#4273 = DIRECTION ( 'NONE',  ( 1.000000000000000000, -3.469446951953602750E-15, 0.000000000000000000 ) ) ;
#4274 = VERTEX_POINT ( 'NONE', #12120 ) ;
#4275 = DIRECTION ( 'NONE',  ( -0.000000000000000000, -0.000000000000000000, 1.000000000000000000 ) ) ;
#4276 = ORIENTED_EDGE ( 'NONE', *, *, #9463, .F. ) ;
#4277 = VERTEX_POINT ( 'NONE', #1656 ) ;
#4278 = MECHANICAL_DESIGN_GEOMETRIC_PRESENTATION_REPRESENTATION (  '', ( #12869 ), #7584 ) ;
#4279 = ORIENTED_EDGE ( 'NONE', *, *, #5730, .F. ) ;
#4280 = VECTOR ( 'NONE', #1928, 1000.000000000000000 ) ;
#4281 = FACE_OUTER_BOUND ( 'NONE', #5664, .T. ) ;
#4282 = VERTEX_POINT ( 'NONE', #617 ) ;
#4283 = CARTESIAN_POINT ( 'NONE',  ( 3.647599401157688437, 3.000000000000000000, 11.52662650599083882 ) ) ;
#4284 = CARTESIAN_POINT ( 'NONE',  ( 10.18987059060247269, 3.000000000000000000, 6.506507307819714647 ) ) ;
#4285 = DIRECTION ( 'NONE',  ( -0.000000000000000000, -1.000000000000000000, -0.000000000000000000 ) ) ;
#4286 = DIRECTION ( 'NONE',  ( -1.000000000000000000, -0.000000000000000000, -0.000000000000000000 ) ) ;
#4287 = EDGE_CURVE ( 'NONE', #5612, #10060, #7071, .T. ) ;
#4288 = CARTESIAN_POINT ( 'NONE',  ( 13.27898586450067242, 3.000000000000000000, -5.170206418547655502 ) ) ;
#4290 = VECTOR ( 'NONE', #12444, 1000.000000000000000 ) ;
#4289 = PRODUCT_DEFINITION ( 'UNKNOWN', '', #581, #2818 ) ;
#4291 = CARTESIAN_POINT ( 'NONE',  ( 31.00000000000000000, 3.000000000000000000, 0.000000000000000000 ) ) ;
#4292 = VECTOR ( 'NONE', #3192, 1000.000000000000000 ) ;
#4293 = DIRECTION ( 'NONE',  ( -0.000000000000000000, -1.000000000000000000, -0.000000000000000000 ) ) ;
#4294 = CARTESIAN_POINT ( 'NONE',  ( -9.065441275458884007, 3.000000000000000000, -9.324917484779556176 ) ) ;
#4295 = ORIENTED_EDGE ( 'NONE', *, *, #11702, .T. ) ;
#4296 = CARTESIAN_POINT ( 'NONE',  ( 12.25282671965375592, 0.000000000000000000, -5.797378255456012930 ) ) ;
#4297 = VERTEX_POINT ( 'NONE', #10943 ) ;
#4298 = B_SPLINE_CURVE_WITH_KNOTS ( 'NONE', 3,
 ( #6368, #4038, #7279, #127 ),
 .UNSPECIFIED., .F., .F.,
 ( 4, 4 ),
 ( 0.000000000000000000, 0.5855695330273008592 ),
 .UNSPECIFIED. ) ;
#4299 = ORIENTED_EDGE ( 'NONE', *, *, #5046, .F. ) ;
#4300 = EDGE_LOOP ( 'NONE', ( #9691, #546, #267, #980 ) ) ;
#4301 = PRESENTATION_LAYER_ASSIGNMENT (  '', '', ( #7172 ) ) ;
#4302 = CIRCLE ( 'NONE', #10463, 3.000000000000000000 ) ;
#4303 = CARTESIAN_POINT ( 'NONE',  ( -5.452638258930639914, 3.000000000000000000, -13.97385902380748313 ) ) ;
#4304 = CARTESIAN_POINT ( 'NONE',  ( 4.355042381134428098, 0.000000000000000000, 7.299562031966232212 ) ) ;
#4305 = EDGE_CURVE ( 'NONE', #3370, #2212, #5846, .T. ) ;
#4306 = EDGE_CURVE ( 'NONE', #10281, #5856, #10139, .T. ) ;
#4307 = CARTESIAN_POINT ( 'NONE',  ( 0.000000000000000000, 3.000000000000000000, 0.000000000000000000 ) ) ;
#4308 = B_SPLINE_CURVE_WITH_KNOTS ( 'NONE', 2,
 ( #12716, #3259, #11676 ),
 .UNSPECIFIED., .F., .F.,
 ( 3, 3 ),
 ( 0.000000000000000000, 1.000000000000000000 ),
 .UNSPECIFIED. ) ;
#4310 = CIRCLE ( 'NONE', #2272, 6.750000000000000888 ) ;
#4309 = CARTESIAN_POINT ( 'NONE',  ( -11.13895890373326836, 3.000000000000000000, 7.723663868796768028 ) ) ;
#4311 = LINE ( 'NONE', #12782, #5738 ) ;
#4312 = ORIENTED_EDGE ( 'NONE', *, *, #2304, .F. ) ;
#4313 = EDGE_CURVE ( 'NONE', #544, #843, #12944, .T. ) ;
#4314 = DIRECTION ( 'NONE',  ( 0.000000000000000000, 0.000000000000000000, 1.000000000000000000 ) ) ;
#4315 = ADVANCED_FACE ( 'NONE', ( #405 ), #11007, .T. ) ;
#4316 = EDGE_LOOP ( 'NONE', ( #10818, #8516, #12803, #10935 ) ) ;
#4317 = VERTEX_POINT ( 'NONE', #6875 ) ;
#4318 = FACE_OUTER_BOUND ( 'NONE', #8137, .T. ) ;
#4319 = ORIENTED_EDGE ( 'NONE', *, *, #13491, .T. ) ;
#4320 = CARTESIAN_POINT ( 'NONE',  ( -12.07793442604884682, 3.000000000000000000, 0.5400000000005513723 ) ) ;
#4321 = EDGE_CURVE ( 'NONE', #12313, #833, #1130, .T. ) ;
#4322 = DIRECTION ( 'NONE',  ( 0.000000000000000000, 0.000000000000000000, 1.000000000000000000 ) ) ;
#4323 = EDGE_CURVE ( 'NONE', #11264, #4866, #13212, .T. ) ;
#4324 = CARTESIAN_POINT ( 'NONE',  ( 6.970598036433451661, 0.000000000000000000, -10.97318381393796294 ) ) ;
#4325 = CARTESIAN_POINT ( 'NONE',  ( 9.573149624528804580, 0.000000000000000000, -8.795158114916638681 ) ) ;
#4326 = DIRECTION ( 'NONE',  ( 0.7216024245882196597, 0.000000000000000000, 0.6923076923076926237 ) ) ;
#4327 = EDGE_CURVE ( 'NONE', #2790, #8976, #4676, .T. ) ;
#4328 = CARTESIAN_POINT ( 'NONE',  ( 7.499999999999999112, 3.000000000000000000, -1.499999999999997780 ) ) ;
#4329 = CARTESIAN_POINT ( 'NONE',  ( 4.227250083625740729, 3.000000000000000000, -13.17831234185050526 ) ) ;
#4330 = B_SPLINE_SURFACE_WITH_KNOTS ( 'NONE', 3, 1, ( 
 ( #12026, #511 ),
 ( #9867, #721 ),
 ( #2708, #10975 ),
 ( #5810, #5881 ) ),
 .UNSPECIFIED., .F., .F., .F.,
 ( 4, 4 ),
 ( 2, 2 ),
 ( 0.000000000000000000, 0.5855695330273008592 ),
 ( 0.000000000000000000, 1.000000000000000000 ),
 .UNSPECIFIED. ) ;
#4331 = ORIENTED_EDGE ( 'NONE', *, *, #10538, .F. ) ;
#4332 = VERTEX_POINT ( 'NONE', #4540 ) ;
#4333 = ORIENTED_EDGE ( 'NONE', *, *, #10954, .F. ) ;
#4334 = DIRECTION ( 'NONE',  ( 0.000000000000000000, 0.000000000000000000, 1.000000000000000000 ) ) ;
#4335 = ORIENTED_EDGE ( 'NONE', *, *, #13266, .F. ) ;
#4336 = EDGE_CURVE ( 'NONE', #3576, #11340, #9972, .T. ) ;
#4337 = EDGE_CURVE ( 'NONE', #544, #11807, #3094, .T. ) ;
#4338 = CARTESIAN_POINT ( 'NONE',  ( -5.977417671213807182, 0.000000000000000000, 3.135757960025121527 ) ) ;
#4339 =( LENGTH_UNIT ( ) NAMED_UNIT ( * ) SI_UNIT ( .MILLI., .METRE. ) );
#4340 = PRODUCT ( 'pin', 'pin', '', ( #13494 ) ) ;
#4341 = CARTESIAN_POINT ( 'NONE',  ( 0.000000000000000000, -3.000000000000000000, 0.000000000000000000 ) ) ;
#4342 = DIRECTION ( 'NONE',  ( -0.000000000000000000, -1.000000000000000000, -0.000000000000000000 ) ) ;
#4343 = CARTESIAN_POINT ( 'NONE',  ( -9.375397774054503586, 0.000000000000000000, -11.70905276178452503 ) ) ;
#4344 = CARTESIAN_POINT ( 'NONE',  ( -11.52662650599092409, 3.000000000000000000, 3.647599401157420651 ) ) ;
#4345 = CARTESIAN_POINT ( 'NONE',  ( -11.70905276178464050, 3.000000000000000000, -9.375397774054366806 ) ) ;
#4346 = ORIENTED_EDGE ( 'NONE', *, *, #1201, .F. ) ;
#4347 = SURFACE_STYLE_USAGE ( .BOTH. , #2409 ) ;
#4348 = ORIENTED_EDGE ( 'NONE', *, *, #10030, .T. ) ;
#4349 = ORIENTED_EDGE ( 'NONE', *, *, #13267, .F. ) ;
#4350 = ORIENTED_EDGE ( 'NONE', *, *, #7532, .T. ) ;
#4351 = CARTESIAN_POINT ( 'NONE',  ( -5.452638258930639914, 3.000000000000000000, -13.97385902380748313 ) ) ;
#4352 = ORIENTED_EDGE ( 'NONE', *, *, #8764, .T. ) ;
#4353 = LINE ( 'NONE', #7519, #6928 ) ;
#4354 = DIRECTION ( 'NONE',  ( 0.000000000000000000, 1.000000000000000000, 0.000000000000000000 ) ) ;
#4355 = CYLINDRICAL_SURFACE ( 'NONE', #11275, 1.500000000000001332 ) ;
#4356 = FACE_OUTER_BOUND ( 'NONE', #3886, .T. ) ;
#4357 = LINE ( 'NONE', #4420, #2002 ) ;
#4358 = CARTESIAN_POINT ( 'NONE',  ( 2.414978278956333213, 3.000000000000000000, -13.33788847341978645 ) ) ;
#4359 = CARTESIAN_POINT ( 'NONE',  ( -0.7527353566742582824, 0.000000000000000000, 7.906594341344654886 ) ) ;
#4360 = CARTESIAN_POINT ( 'NONE',  ( -3.835481108877868195, 9.000000000000000000, 5.554420281491219136 ) ) ;
#4361 = ORIENTED_EDGE ( 'NONE', *, *, #8708, .F. ) ;
#4362 = CARTESIAN_POINT ( 'NONE',  ( -3.647470871583628593, 0.000000000000000000, 11.52666717836884125 ) ) ;
#4363 = EDGE_LOOP ( 'NONE', ( #12189, #3255, #5453, #9314 ) ) ;
#4364 = EDGE_LOOP ( 'NONE', ( #5842, #6372, #10186, #10436 ) ) ;
#4365 = EDGE_CURVE ( 'NONE', #7906, #6233, #6538, .T. ) ;
#4366 = ORIENTED_EDGE ( 'NONE', *, *, #4706, .F. ) ;
#4367 = CARTESIAN_POINT ( 'NONE',  ( -12.98835496148299207, 0.000000000000000000, 0.5501230721524459355 ) ) ;
#4368 = CARTESIAN_POINT ( 'NONE',  ( -1.557181465540221188, 0.000000000000000000, 14.16466328168015743 ) ) ;
#4369 = CARTESIAN_POINT ( 'NONE',  ( 11.14709020439929787, 0.000000000000000000, 7.712570079660892475 ) ) ;
#4370 = CARTESIAN_POINT ( 'NONE',  ( 0.000000000000000000, 9.000000000000000000, -6.750000000000000888 ) ) ;
#4371 = DIRECTION ( 'NONE',  ( 0.000000000000000000, 1.000000000000000000, -0.000000000000000000 ) ) ;
#4372 = CARTESIAN_POINT ( 'NONE',  ( -2.161962830978702677, 3.000000000000000000, 14.08504230442587435 ) ) ;
#4373 = VECTOR ( 'NONE', #4892, 1000.000000000000000 ) ;
#4374 = ORIENTED_EDGE ( 'NONE', *, *, #2060, .F. ) ;
#4375 = ORIENTED_EDGE ( 'NONE', *, *, #13136, .T. ) ;
#4376 = EDGE_CURVE ( 'NONE', #7949, #10891, #11470, .T. ) ;
#4377 = FACE_OUTER_BOUND ( 'NONE', #7770, .T. ) ;
#4378 = EDGE_CURVE ( 'NONE', #1810, #1061, #8789, .T. ) ;
#4379 = VERTEX_POINT ( 'NONE', #9361 ) ;
#4380 = CARTESIAN_POINT ( 'NONE',  ( -21.21140389626389222, 3.000000000000000000, 12.49772878833445056 ) ) ;
#4381 = EDGE_CURVE ( 'NONE', #2083, #1162, #9692, .T. ) ;
#4382 = CARTESIAN_POINT ( 'NONE',  ( 0.000000000000000000, 3.000000000000000000, 0.000000000000000000 ) ) ;
#4383 = DIRECTION ( 'NONE',  ( 0.000000000000000000, 1.000000000000000000, 0.000000000000000000 ) ) ;
#4384 = CARTESIAN_POINT ( 'NONE',  ( 4.690415759823430619, 2.900000000000000355, -1.399999999999999911 ) ) ;
#4385 = VECTOR ( 'NONE', #8788, 1000.000000000000000 ) ;
#4386 = LINE ( 'NONE', #1287, #6039 ) ;
#4387 = CARTESIAN_POINT ( 'NONE',  ( 47.14458624375820506, 3.000000000000000000, -3.829406728833672613 ) ) ;
#4388 = CARTESIAN_POINT ( 'NONE',  ( 5.170206418547656391, 0.000000000000000000, 13.27898586450067064 ) ) ;
#4389 = ADVANCED_FACE ( 'NONE', ( #10256 ), #9210, .T. ) ;
#4390 = VERTEX_POINT ( 'NONE', #12196 ) ;
#4391 = EDGE_LOOP ( 'NONE', ( #6804, #11958, #5166, #1498 ) ) ;
#4392 = ORIENTED_EDGE ( 'NONE', *, *, #1631, .T. ) ;
#4393 = FACE_OUTER_BOUND ( 'NONE', #147, .T. ) ;
#4394 = AXIS2_PLACEMENT_3D ( 'NONE', #2170, #11613, #6239 ) ;
#4395 = CIRCLE ( 'NONE', #12763, 1.500000000000000444 ) ;
#4396 = ORIENTED_EDGE ( 'NONE', *, *, #8629, .T. ) ;
#4397 = ADVANCED_FACE ( 'NONE', ( #3907 ), #11620, .F. ) ;
#4398 = EDGE_CURVE ( 'NONE', #3759, #5524, #9284, .T. ) ;
#4399 = FACE_OUTER_BOUND ( 'NONE', #4206, .T. ) ;
#4400 = DIRECTION ( 'NONE',  ( 0.000000000000000000, 0.000000000000000000, 1.000000000000000000 ) ) ;
#4401 = CARTESIAN_POINT ( 'NONE',  ( 0.000000000000000000, 0.000000000000000000, 0.000000000000000000 ) ) ;
#4402 = DIRECTION ( 'NONE',  ( -0.000000000000000000, -1.000000000000000000, 0.000000000000000000 ) ) ;
#4403 = AXIS2_PLACEMENT_3D ( 'NONE', #11454, #8084, #10427 ) ;
#4404 = APPLICATION_CONTEXT ( 'automotive_design' ) ;
#4405 = CARTESIAN_POINT ( 'NONE',  ( -12.56087513340552242, 0.000000000000000000, 2.568302020731519253 ) ) ;
#4406 = CARTESIAN_POINT ( 'NONE',  ( -12.40340517008309185, 3.000000000000000000, -3.893011711613028947 ) ) ;
#4407 = ORIENTED_EDGE ( 'NONE', *, *, #8491, .F. ) ;
#4408 = DIRECTION ( 'NONE',  ( -0.000000000000000000, -1.000000000000000000, -0.000000000000000000 ) ) ;
#4409 = ORIENTED_EDGE ( 'NONE', *, *, #10627, .F. ) ;
#4410 = EDGE_CURVE ( 'NONE', #5397, #1515, #2005, .T. ) ;
#4411 = EDGE_LOOP ( 'NONE', ( #12133, #5226 ) ) ;
#4412 = EDGE_LOOP ( 'NONE', ( #3406, #5009, #2985, #11712 ) ) ;
#4413 = CARTESIAN_POINT ( 'NONE',  ( -12.98835496148299207, 0.000000000000000000, 0.5501230721524460465 ) ) ;
#4414 = ORIENTED_EDGE ( 'NONE', *, *, #12477, .T. ) ;
#4415 = VECTOR ( 'NONE', #10863, 1000.000000000000000 ) ;
#4416 = AXIS2_PLACEMENT_3D ( 'NONE', #1578, #4749, #2670 ) ;
#4417 = DIRECTION ( 'NONE',  ( -0.000000000000000000, -1.000000000000000000, -0.000000000000000000 ) ) ;
#4418 = CARTESIAN_POINT ( 'NONE',  ( -0.8123631076467130452, 9.000000000000000000, -6.700937709107179785 ) ) ;
#4419 = CARTESIAN_POINT ( 'NONE',  ( 0.000000000000000000, 9.000000000000000000, -6.750000000000000888 ) ) ;
#4420 = CARTESIAN_POINT ( 'NONE',  ( 20.00000000000000355, 3.000000000000000000, -14.92471123914604370 ) ) ;
#4421 = DIRECTION ( 'NONE',  ( 0.000000000000000000, -0.000000000000000000, -1.000000000000000000 ) ) ;
#4422 = DIRECTION ( 'NONE',  ( 0.000000000000000000, 0.000000000000000000, -1.000000000000000000 ) ) ;
#4423 = DIRECTION ( 'NONE',  ( 0.000000000000000000, 0.000000000000000000, 1.000000000000000000 ) ) ;
#4424 = EDGE_LOOP ( 'NONE', ( #7431, #7570, #10921, #12591 ) ) ;
#4425 = CARTESIAN_POINT ( 'NONE',  ( 2.392396671352952087, 9.000000000000000000, 6.311809420990097230 ) ) ;
#4426 = CIRCLE ( 'NONE', #9263, 2.999999999999999112 ) ;
#4427 = EDGE_CURVE ( 'NONE', #11094, #5187, #4874, .T. ) ;
#4428 = VECTOR ( 'NONE', #9936, 1000.000000000000000 ) ;
#4429 = ORIENTED_EDGE ( 'NONE', *, *, #7588, .F. ) ;
#4430 = ADVANCED_FACE ( 'NONE', ( #3977 ), #11215, .F. ) ;
#4431 = EDGE_LOOP ( 'NONE', ( #2661, #13080 ) ) ;
#4432 = EDGE_LOOP ( 'NONE', ( #5325, #3888, #2128, #4075 ) ) ;
#4433 = CARTESIAN_POINT ( 'NONE',  ( -10.88404822699983576, 3.000000000000000000, 29.60989680561421622 ) ) ;
#4434 = LINE ( 'NONE', #6709, #13304 ) ;
#4435 = AXIS2_PLACEMENT_3D ( 'NONE', #6626, #11936, #4422 ) ;
#4436 = CARTESIAN_POINT ( 'NONE',  ( -8.369528376005813897, 9.000000000000000000, 1.483574994138652903 ) ) ;
#4437 = CYLINDRICAL_SURFACE ( 'NONE', #11684, 1.500000000000000222 ) ;
#4438 = CARTESIAN_POINT ( 'NONE',  ( -2.604531154829235362, 0.000000000000000000, -11.80612203322752585 ) ) ;
#4439 = CARTESIAN_POINT ( 'NONE',  ( 10.00000000000001243, 5.000000000000006217, 10.00000000000000178 ) ) ;
#4440 = ORIENTED_EDGE ( 'NONE', *, *, #707, .F. ) ;
#4441 = AXIS2_PLACEMENT_3D ( 'NONE', #2868, #13555, #8367 ) ;
#4442 = VERTEX_POINT ( 'NONE', #886 ) ;
#4443 = CARTESIAN_POINT ( 'NONE',  ( 4.227250083625740729, 3.000000000000000000, -13.17831234185050526 ) ) ;
#4444 = B_SPLINE_SURFACE_WITH_KNOTS ( 'NONE', 3, 1, ( 
 ( #10884, #1449 ),
 ( #5639, #9836 ),
 ( #408, #4606 ),
 ( #9549, #9153 ) ),
 .UNSPECIFIED., .F., .F., .F.,
 ( 4, 4 ),
 ( 2, 2 ),
 ( 0.1547128134717859205, 1.000000000000000000 ),
 ( 0.000000000000000000, 1.000000000000000000 ),
 .UNSPECIFIED. ) ;
#4445 = ORIENTED_EDGE ( 'NONE', *, *, #5021, .T. ) ;
#4446 = CARTESIAN_POINT ( 'NONE',  ( -14.87484884897978077, 0.000000000000000000, -1.958311002203079187 ) ) ;
#4447 = DIRECTION ( 'NONE',  ( 0.000000000000000000, 0.000000000000000000, -1.000000000000000000 ) ) ;
#4448 = CIRCLE ( 'NONE', #8397, 2.999999999999999112 ) ;
#4449 = AXIS2_PLACEMENT_3D ( 'NONE', #11173, #5933, #1534 ) ;
#4450 = DIRECTION ( 'NONE',  ( 0.000000000000000000, -1.000000000000000000, 0.000000000000000000 ) ) ;
#4451 = DIRECTION ( 'NONE',  ( 0.000000000000000000, 1.000000000000000000, 0.000000000000000000 ) ) ;
#4452 = EDGE_CURVE ( 'NONE', #5502, #6360, #3240, .T. ) ;
#4453 = CARTESIAN_POINT ( 'NONE',  ( -13.04554897075799680, 3.000000000000000000, -5.733772933379471581 ) ) ;
#4454 = CYLINDRICAL_SURFACE ( 'NONE', #10661, 1.500000000000000666 ) ;
#4455 = CARTESIAN_POINT ( 'NONE',  ( 1.105736515254441388, 0.000000000000000000, -13.50994833511691695 ) ) ;
#4456 = ORIENTED_EDGE ( 'NONE', *, *, #31, .T. ) ;
#4457 = VERTEX_POINT ( 'NONE', #1721 ) ;
#4458 = EDGE_LOOP ( 'NONE', ( #7842, #25, #4864, #13544 ) ) ;
#4459 = AXIS2_PLACEMENT_3D ( 'NONE', #12423, #10397, #898 ) ;
#4460 = ORIENTED_EDGE ( 'NONE', *, *, #3473, .T. ) ;
#4461 = DIRECTION ( 'NONE',  ( 0.000000000000000000, 1.000000000000000000, 0.000000000000000000 ) ) ;
#4462 = AXIS2_PLACEMENT_3D ( 'NONE', #4307, #7818, #1011 ) ;
#4463 =( GEOMETRIC_REPRESENTATION_CONTEXT ( 3 ) GLOBAL_UNCERTAINTY_ASSIGNED_CONTEXT ( ( #480 ) ) GLOBAL_UNIT_ASSIGNED_CONTEXT ( ( #13297, #8057, #1454 ) ) REPRESENTATION_CONTEXT ( 'NONE', 'WORKASPACE' ) );
#4464 = ORIENTED_EDGE ( 'NONE', *, *, #8297, .F. ) ;
#4465 = DIRECTION ( 'NONE',  ( -1.000000000000000000, 0.000000000000000000, 0.000000000000000000 ) ) ;
#4466 = SHAPE_REPRESENTATION_RELATIONSHIP ( 'NONE' , 'NONE' ,  #8461, #12787 ) ;
#4467 = EDGE_CURVE ( 'NONE', #11339, #2737, #12125, .T. ) ;
#4468 = CARTESIAN_POINT ( 'NONE',  ( 5.708888906988906164, 0.000000000000000000, -11.46847481510586775 ) ) ;
#4469 = B_SPLINE_CURVE_WITH_KNOTS ( 'NONE', 3,
 ( #2449, #12793, #8569, #3339 ),
 .UNSPECIFIED., .F., .F.,
 ( 4, 4 ),
 ( 0.000000000000000000, 0.8452273900860258760 ),
 .UNSPECIFIED. ) ;
#4470 = EDGE_CURVE ( 'NONE', #12047, #1815, #10105, .T. ) ;
#4471 = AXIS2_PLACEMENT_3D ( 'NONE', #2243, #12665, #6452 ) ;
#4472 = DIRECTION ( 'NONE',  ( 0.000000000000000000, -1.000000000000000000, 0.000000000000000000 ) ) ;
#4473 = B_SPLINE_CURVE_WITH_KNOTS ( 'NONE', 2,
 ( #2313, #6510, #12855 ),
 .UNSPECIFIED., .F., .F.,
 ( 3, 3 ),
 ( 0.000000000000000000, 1.000000000000000000 ),
 .UNSPECIFIED. ) ;
#4474 = AXIS2_PLACEMENT_3D ( 'NONE', #11456, #107, #5119 ) ;
#4475 = MECHANICAL_DESIGN_GEOMETRIC_PRESENTATION_REPRESENTATION (  '', ( #9093 ), #11743 ) ;
#4476 = CARTESIAN_POINT ( 'NONE',  ( 9.133371500908369356, 0.000000000000000000, -11.90284147956862171 ) ) ;
#4477 = DIRECTION ( 'NONE',  ( -0.000000000000000000, -1.000000000000000000, -0.000000000000000000 ) ) ;
#4478 = ORIENTED_EDGE ( 'NONE', *, *, #3005, .F. ) ;
#4479 = ADVANCED_FACE ( 'NONE', ( #7019 ), #4241, .F. ) ;
#4480 = CARTESIAN_POINT ( 'NONE',  ( -4.499999999999993783, 3.000000000000000000, 13.39999999999999858 ) ) ;
#4481 = EDGE_LOOP ( 'NONE', ( #6117, #10887, #13039, #3776 ) ) ;
#4482 = EDGE_CURVE ( 'NONE', #13298, #12936, #4857, .T. ) ;
#4483 = ORIENTED_EDGE ( 'NONE', *, *, #3358, .F. ) ;
#4484 = ORIENTED_EDGE ( 'NONE', *, *, #4100, .T. ) ;
#4485 = CARTESIAN_POINT ( 'NONE',  ( 12.63269908545826503, 3.000000000000000000, -5.340493616518843467 ) ) ;
#4486 = ORIENTED_EDGE ( 'NONE', *, *, #5965, .F. ) ;
#4487 = AXIS2_PLACEMENT_3D ( 'NONE', #11642, #10682, #6398 ) ;
#4488 = ORIENTED_EDGE ( 'NONE', *, *, #9258, .F. ) ;
#4489 = CIRCLE ( 'NONE', #13075, 8.499999999999998224 ) ;
#4490 = DIRECTION ( 'NONE',  ( -1.000000000000000000, 0.000000000000000000, 0.000000000000000000 ) ) ;
#4491 = CARTESIAN_POINT ( 'NONE',  ( 26.30958424017656938, 2.900000000000000355, 4.500000000000000888 ) ) ;
#4492 = EDGE_CURVE ( 'NONE', #7043, #11145, #3848, .T. ) ;
#4493 = DIRECTION ( 'NONE',  ( 0.000000000000000000, 1.000000000000000000, 0.000000000000000000 ) ) ;
#4494 = CARTESIAN_POINT ( 'NONE',  ( -13.49999999999999645, 3.000000000000000000, -5.549999999999999822 ) ) ;
#4495 = CARTESIAN_POINT ( 'NONE',  ( -10.33484986938308303, 3.000000000000000000, 8.771102293099071190 ) ) ;
#4496 = DIRECTION ( 'NONE',  ( -1.000000000000000000, 0.000000000000000000, 1.370446048119726253E-16 ) ) ;
#4497 = ORIENTED_EDGE ( 'NONE', *, *, #8585, .F. ) ;
#4498 = AXIS2_PLACEMENT_3D ( 'NONE', #7817, #7880, #4728 ) ;
#4499 = FACE_OUTER_BOUND ( 'NONE', #3929, .T. ) ;
#4500 = VECTOR ( 'NONE', #13150, 1000.000000000000000 ) ;
#4501 = ADVANCED_FACE ( 'NONE', ( #5979 ), #5281, .F. ) ;
#4502 = EDGE_LOOP ( 'NONE', ( #6162, #6163, #11562, #1182 ) ) ;
#4503 = ORIENTED_EDGE ( 'NONE', *, *, #2557, .F. ) ;
#4504 = ORIENTED_EDGE ( 'NONE', *, *, #9144, .T. ) ;
#4505 = CARTESIAN_POINT ( 'NONE',  ( -14.90895795148409420, 3.000000000000000000, 1.650143266773909101 ) ) ;
#4506 = VECTOR ( 'NONE', #9805, 1000.000000000000000 ) ;
#4507 = AXIS2_PLACEMENT_3D ( 'NONE', #12290, #11240, #9099 ) ;
#4508 = DIRECTION ( 'NONE',  ( -0.000000000000000000, -1.000000000000000000, -0.000000000000000000 ) ) ;
#4509 = EDGE_CURVE ( 'NONE', #1456, #868, #8558, .T. ) ;
#4510 = EDGE_CURVE ( 'NONE', #2370, #4741, #9419, .T. ) ;
#4511 = CARTESIAN_POINT ( 'NONE',  ( 28.54655175640005282, 0.000000000000000000, 2.353846153846155254 ) ) ;
#4512 = CARTESIAN_POINT ( 'NONE',  ( -8.795158114916672432, 3.000000000000000000, -9.573149624528774382 ) ) ;
#4513 = CARTESIAN_POINT ( 'NONE',  ( 4.690415759823430619, 0.1000000000000000056, 1.399999999999999911 ) ) ;
#4514 = CARTESIAN_POINT ( 'NONE',  ( 0.000000000000000000, 3.000000000000000000, 0.000000000000000000 ) ) ;
#4515 = ORIENTED_EDGE ( 'NONE', *, *, #613, .T. ) ;
#4516 = AXIS2_PLACEMENT_3D ( 'NONE', #5042, #6909, #9242 ) ;
#4517 = TOROIDAL_SURFACE ( 'NONE', #1218, 3.399999999999999911, 0.1000000000000000056 ) ;
#4518 = ORIENTED_EDGE ( 'NONE', *, *, #1256, .T. ) ;
#4519 = DIRECTION ( 'NONE',  ( 0.000000000000000000, 0.000000000000000000, -1.000000000000000000 ) ) ;
#4520 = EDGE_LOOP ( 'NONE', ( #6322, #8328, #4429, #193 ) ) ;
#4521 = DIRECTION ( 'NONE',  ( 0.7772490812545727046, 0.000000000000000000, 0.6291930273683288277 ) ) ;
#4522 = B_SPLINE_SURFACE_WITH_KNOTS ( 'NONE', 2, 1, ( 
 ( #8711, #12928 ),
 ( #8506, #3267 ),
 ( #6580, #12726 ) ),
 .UNSPECIFIED., .F., .F., .F.,
 ( 3, 3 ),
 ( 2, 2 ),
 ( 0.000000000000000000, 0.02941149433826504428 ),
 ( 0.000000000000000000, 1.000000000000000000 ),
 .UNSPECIFIED. ) ;
#4523 =( GEOMETRIC_REPRESENTATION_CONTEXT ( 3 ) GLOBAL_UNCERTAINTY_ASSIGNED_CONTEXT ( ( #5578 ) ) GLOBAL_UNIT_ASSIGNED_CONTEXT ( ( #4339, #12686, #1098 ) ) REPRESENTATION_CONTEXT ( 'NONE', 'WORKASPACE' ) );
#4524 = CARTESIAN_POINT ( 'NONE',  ( 31.00000000000000000, 0.09999999999999982514, 0.000000000000000000 ) ) ;
#4525 = CARTESIAN_POINT ( 'NONE',  ( 0.5501230721522984979, 3.000000000000000000, -12.98835496148321766 ) ) ;
#4526 = CARTESIAN_POINT ( 'NONE',  ( 6.553553527263006551, 9.000000000000000000, 1.616612558808879774 ) ) ;
#4527 = CARTESIAN_POINT ( 'NONE',  ( -5.299649803506881085, 9.000000000000000000, -6.645578376649351249 ) ) ;
#4528 = CARTESIAN_POINT ( 'NONE',  ( 8.093005444143644311, 0.000000000000000000, -2.598704077239528232 ) ) ;
#4529 = DIRECTION ( 'NONE',  ( -0.000000000000000000, -1.000000000000000000, -0.000000000000000000 ) ) ;
#4530 = ORIENTED_EDGE ( 'NONE', *, *, #6673, .F. ) ;
#4531 = ORIENTED_EDGE ( 'NONE', *, *, #9798, .T. ) ;
#4532 = VERTEX_POINT ( 'NONE', #4117 ) ;
#4533 = AXIS2_PLACEMENT_3D ( 'NONE', #4178, #316, #12853 ) ;
#4534 = ORIENTED_EDGE ( 'NONE', *, *, #3731, .F. ) ;
#4535 = DIRECTION ( 'NONE',  ( -0.000000000000000000, -1.000000000000000000, -0.000000000000000000 ) ) ;
#4536 = EDGE_CURVE ( 'NONE', #6360, #9461, #3534, .T. ) ;
#4537 = ORIENTED_EDGE ( 'NONE', *, *, #1057, .T. ) ;
#4538 = CARTESIAN_POINT ( 'NONE',  ( -6.549210654805285081, 9.000000000000000000, 1.634117437329677180 ) ) ;
#4539 = CARTESIAN_POINT ( 'NONE',  ( 0.000000000000000000, 0.000000000000000000, 0.000000000000000000 ) ) ;
#4540 = CARTESIAN_POINT ( 'NONE',  ( 6.749972395921142621, 0.000000000000000000, -0.01930425607464712062 ) ) ;
#4541 = LINE ( 'NONE', #6679, #318 ) ;
#4542 = FACE_OUTER_BOUND ( 'NONE', #9778, .T. ) ;
#4543 = CARTESIAN_POINT ( 'NONE',  ( -13.97385902380755240, 3.000000000000000000, -5.452638258930474713 ) ) ;
#4544 = ORIENTED_EDGE ( 'NONE', *, *, #2196, .T. ) ;
#4545 = CYLINDRICAL_SURFACE ( 'NONE', #7126, 3.000000000000000000 ) ;
#4546 = ORIENTED_EDGE ( 'NONE', *, *, #2379, .F. ) ;
#4547 = ORIENTED_EDGE ( 'NONE', *, *, #8931, .F. ) ;
#4548 = ORIENTED_EDGE ( 'NONE', *, *, #9812, .F. ) ;
#4549 = CARTESIAN_POINT ( 'NONE',  ( -1.604252589105048976, 9.000000000000000000, -8.347237484961699039 ) ) ;
#4550 = EDGE_CURVE ( 'NONE', #2353, #4598, #5078, .T. ) ;
#4551 = ADVANCED_FACE ( 'NONE', ( #9483, #1024 ), #3269, .F. ) ;
#4552 = ORIENTED_EDGE ( 'NONE', *, *, #11879, .F. ) ;
#4553 = ORIENTED_EDGE ( 'NONE', *, *, #6010, .T. ) ;
#4554 = DIRECTION ( 'NONE',  ( -0.000000000000000000, -1.000000000000000000, -0.000000000000000000 ) ) ;
#4555 = FILL_AREA_STYLE_COLOUR ( '', #7803 ) ;
#4556 = EDGE_CURVE ( 'NONE', #9203, #10050, #10727, .T. ) ;
#4557 = CARTESIAN_POINT ( 'NONE',  ( 2.161962830978694683, 3.000000000000000000, -14.08504230442587790 ) ) ;
#4558 = CARTESIAN_POINT ( 'NONE',  ( 8.883544964651964193, 3.000000000000000000, -12.08646469655236544 ) ) ;
#4559 = B_SPLINE_CURVE_WITH_KNOTS ( 'NONE', 3,
 ( #6574, #8704, #2582, #12920 ),
 .UNSPECIFIED., .F., .F.,
 ( 4, 4 ),
 ( 0.000000000000000000, 0.5855695330273008592 ),
 .UNSPECIFIED. ) ;
#4560 = LINE ( 'NONE', #422, #2946 ) ;
#4561 = CARTESIAN_POINT ( 'NONE',  ( 8.922136023539611216, 3.000000000000000000, -8.158651161643899030 ) ) ;
#4562 = CARTESIAN_POINT ( 'NONE',  ( -14.39763212228012534, 0.000000000000000000, 1.133238802859812155 ) ) ;
#4563 = ORIENTED_EDGE ( 'NONE', *, *, #8504, .T. ) ;
#4564 = CARTESIAN_POINT ( 'NONE',  ( 5.504794476853524188, 0.000000000000000000, -4.890042597913815570 ) ) ;
#4565 = B_SPLINE_SURFACE_WITH_KNOTS ( 'NONE', 3, 1, ( 
 ( #7242, #1941 ),
 ( #6074, #11584 ),
 ( #9434, #3169 ),
 ( #11436, #8391 ) ),
 .UNSPECIFIED., .F., .F., .F.,
 ( 4, 4 ),
 ( 2, 2 ),
 ( 0.000000000000000000, 0.5855695330273008592 ),
 ( 0.000000000000000000, 1.000000000000000000 ),
 .UNSPECIFIED. ) ;
#4566 = VERTEX_POINT ( 'NONE', #11490 ) ;
#4567 = VERTEX_POINT ( 'NONE', #10666 ) ;
#4568 = EDGE_CURVE ( 'NONE', #5777, #9675, #11903, .T. ) ;
#4569 = ORIENTED_EDGE ( 'NONE', *, *, #11808, .F. ) ;
#4570 = LINE ( 'NONE', #6706, #2076 ) ;
#4571 = CARTESIAN_POINT ( 'NONE',  ( 5.170206418547588001, 0.000000000000000000, -13.27898586450069907 ) ) ;
#4572 = EDGE_CURVE ( 'NONE', #4442, #13298, #2057, .T. ) ;
#4573 = ITEM_DEFINED_TRANSFORMATION ( 'NONE', 'NONE', #9803,  #10007 ) ;
#4574 = FACE_OUTER_BOUND ( 'NONE', #6923, .T. ) ;
#4575 = CARTESIAN_POINT ( 'NONE',  ( -9.573149624528719315, 0.000000000000000000, -8.795158114916407754 ) ) ;
#4576 = DIRECTION ( 'NONE',  ( 0.000000000000000000, 0.000000000000000000, 1.000000000000000000 ) ) ;
#4577 = CARTESIAN_POINT ( 'NONE',  ( 1.836970198721030181E-16, 3.000000000000000000, 1.500000000000000222 ) ) ;
#4578 = ORIENTED_EDGE ( 'NONE', *, *, #1274, .F. ) ;
#4579 = ORIENTED_EDGE ( 'NONE', *, *, #7221, .F. ) ;
#4580 = EDGE_CURVE ( 'NONE', #13415, #7348, #9904, .T. ) ;
#4581 = FACE_OUTER_BOUND ( 'NONE', #11370, .T. ) ;
#4582 = EDGE_CURVE ( 'NONE', #8184, #10069, #273, .T. ) ;
#4583 = B_SPLINE_CURVE_WITH_KNOTS ( 'NONE', 3,
 ( #7900, #5849, #13152, #8869 ),
 .UNSPECIFIED., .F., .F.,
 ( 4, 4 ),
 ( 0.2727224849193458089, 0.3021405619770169415 ),
 .UNSPECIFIED. ) ;
#4584 = B_SPLINE_CURVE_WITH_KNOTS ( 'NONE', 3,
 ( #6105, #13405, #6165, #3063 ),
 .UNSPECIFIED., .F., .F.,
 ( 4, 4 ),
 ( 0.000000000000000000, 0.5855695330273008592 ),
 .UNSPECIFIED. ) ;
#4585 = ORIENTED_EDGE ( 'NONE', *, *, #13097, .F. ) ;
#4586 = DIRECTION ( 'NONE',  ( 0.000000000000000000, 0.000000000000000000, 1.000000000000000000 ) ) ;
#4587 = CARTESIAN_POINT ( 'NONE',  ( 2.453448243599949397, 3.000000000000000000, 2.353846153846154365 ) ) ;
#4588 = CARTESIAN_POINT ( 'NONE',  ( 6.017756925049591921, 0.000000000000000000, -11.52330688609011844 ) ) ;
#4589 = FACE_OUTER_BOUND ( 'NONE', #7187, .T. ) ;
#4590 = DIRECTION ( 'NONE',  ( 0.000000000000000000, 0.000000000000000000, 1.000000000000000000 ) ) ;
#4591 = CARTESIAN_POINT ( 'NONE',  ( -11.90209577080766046, 0.000000000000000000, -8.180229652970757215 ) ) ;
#4592 = CARTESIAN_POINT ( 'NONE',  ( 31.00000000000000000, 3.000000000000000000, -1.073670993220974656E-09 ) ) ;
#4593 = CARTESIAN_POINT ( 'NONE',  ( 8.771102293099069414, 0.000000000000000000, 10.33484986938308303 ) ) ;
#4594 = ORIENTED_EDGE ( 'NONE', *, *, #12810, .F. ) ;
#4595 = EDGE_CURVE ( 'NONE', #7175, #10532, #5298, .T. ) ;
#4596 = ORIENTED_EDGE ( 'NONE', *, *, #11489, .T. ) ;
#4597 = EDGE_CURVE ( 'NONE', #8655, #9873, #12670, .T. ) ;
#4598 = VERTEX_POINT ( 'NONE', #4250 ) ;
#4599 = ORIENTED_EDGE ( 'NONE', *, *, #2799, .T. ) ;
#4600 = CARTESIAN_POINT ( 'NONE',  ( 5.985774866078160450, 0.000000000000000000, 3.119775513178307147 ) ) ;
#4601 = ORIENTED_EDGE ( 'NONE', *, *, #13551, .F. ) ;
#4602 = AXIS2_PLACEMENT_3D ( 'NONE', #4249, #1986, #8309 ) ;
#4603 = DIRECTION ( 'NONE',  ( 0.000000000000000000, -1.000000000000000000, 0.000000000000000000 ) ) ;
#4604 = CARTESIAN_POINT ( 'NONE',  ( -11.11702303352197063, 0.000000000000000000, -8.914835885878215294 ) ) ;
#4605 = DIRECTION ( 'NONE',  ( 0.000000000000000000, 0.000000000000000000, -1.000000000000000000 ) ) ;
#4606 = CARTESIAN_POINT ( 'NONE',  ( 8.760376775873721655, 0.000000000000000000, -10.34346111134700585 ) ) ;
#4607 = CYLINDRICAL_SURFACE ( 'NONE', #1443, 0.9999999999999991118 ) ;
#4608 = EDGE_LOOP ( 'NONE', ( #612, #10566, #3646, #7173 ) ) ;
#4609 = CARTESIAN_POINT ( 'NONE',  ( -5.797378255456022700, 3.000000000000000000, -12.25282671965375592 ) ) ;
#4610 = EDGE_LOOP ( 'NONE', ( #3914, #6530, #4530, #2350 ) ) ;
#4611 = VECTOR ( 'NONE', #8903, 1000.000000000000000 ) ;
#4612 = ORIENTED_EDGE ( 'NONE', *, *, #3113, .T. ) ;
#4613 = DIRECTION ( 'NONE',  ( -0.000000000000000000, -1.000000000000000000, -0.000000000000000000 ) ) ;
#4614 = ORIENTED_EDGE ( 'NONE', *, *, #3200, .F. ) ;
#4615 = ORIENTED_EDGE ( 'NONE', *, *, #11492, .T. ) ;
#4616 = CARTESIAN_POINT ( 'NONE',  ( 30.80713437936438126, 3.000000000000000000, 0.9994049933487144655 ) ) ;
#4617 = AXIS2_PLACEMENT_3D ( 'NONE', #1621, #5816, #10014 ) ;
#4618 = CARTESIAN_POINT ( 'NONE',  ( -11.52330688609014686, 0.000000000000000000, -6.017756925049552841 ) ) ;
#4619 = SURFACE_STYLE_FILL_AREA ( #9917 ) ;
#4620 = VECTOR ( 'NONE', #298, 1000.000000000000000 ) ;
#4621 = DIRECTION ( 'NONE',  ( -0.000000000000000000, -1.000000000000000000, -0.000000000000000000 ) ) ;
#4622 = CARTESIAN_POINT ( 'NONE',  ( -5.065227977808755000, 9.000000000000000000, -4.461610195077942542 ) ) ;
#4623 = CYLINDRICAL_SURFACE ( 'NONE', #8893, 3.000000000000000888 ) ;
#4624 = ADVANCED_FACE ( 'NONE', ( #12729 ), #7438, .F. ) ;
#4625 = VERTEX_POINT ( 'NONE', #5218 ) ;
#4626 = EDGE_CURVE ( 'NONE', #2353, #2068, #4179, .T. ) ;
#4627 = CARTESIAN_POINT ( 'NONE',  ( 6.017756925049591921, 3.000000000000000000, -11.52330688609011844 ) ) ;
#4628 = ORIENTED_EDGE ( 'NONE', *, *, #1057, .F. ) ;
#4629 = ORIENTED_EDGE ( 'NONE', *, *, #5312, .F. ) ;
#4630 = CIRCLE ( 'NONE', #7704, 2.500000000000000000 ) ;
#4631 = CIRCLE ( 'NONE', #27, 9.250000000000000000 ) ;
#4632 = VERTEX_POINT ( 'NONE', #8446 ) ;
#4633 = DIRECTION ( 'NONE',  ( 2.602085213965210149E-16, -0.000000000000000000, 1.000000000000000000 ) ) ;
#4634 = CARTESIAN_POINT ( 'NONE',  ( 5.170206418547588001, 3.000000000000000000, -13.27898586450069907 ) ) ;
#4635 = DIRECTION ( 'NONE',  ( 0.000000000000000000, 1.000000000000000000, -0.000000000000000000 ) ) ;
#4636 = CARTESIAN_POINT ( 'NONE',  ( -12.08646469655240097, 3.000000000000000000, -8.883544964651921561 ) ) ;
#4637 = CONTEXT_DEPENDENT_SHAPE_REPRESENTATION ( #7665, #11846 ) ;
#4638 = DIRECTION ( 'NONE',  ( -0.000000000000000000, -1.000000000000000000, -0.000000000000000000 ) ) ;
#4639 = ADVANCED_FACE ( 'NONE', ( #6379 ), #10591, .T. ) ;
#4640 = CARTESIAN_POINT ( 'NONE',  ( -9.573149624528719315, 3.000000000000000000, -8.795158114916407754 ) ) ;
#4641 = CARTESIAN_POINT ( 'NONE',  ( 5.731782959214990036, 3.000000000000000000, 11.46814821560793618 ) ) ;
#4642 = AXIS2_PLACEMENT_3D ( 'NONE', #6799, #5697, #5637 ) ;
#4643 = ADVANCED_FACE ( 'NONE', ( #10786 ), #9527, .T. ) ;
#4644 = FACE_OUTER_BOUND ( 'NONE', #5360, .T. ) ;
#4645 = VERTEX_POINT ( 'NONE', #2525 ) ;
#4646 = EDGE_CURVE ( 'NONE', #8355, #3822, #4732, .T. ) ;
#4647 = ORIENTED_EDGE ( 'NONE', *, *, #12925, .F. ) ;
#4648 = EDGE_CURVE ( 'NONE', #6867, #11838, #12104, .T. ) ;
#4649 = VECTOR ( 'NONE', #9397, 1000.000000000000000 ) ;
#4650 = EDGE_LOOP ( 'NONE', ( #6464, #10617, #57, #4504 ) ) ;
#4651 = DIRECTION ( 'NONE',  ( -0.000000000000000000, -1.000000000000000000, 0.000000000000000000 ) ) ;
#4652 = CYLINDRICAL_SURFACE ( 'NONE', #7572, 1.000000000000000888 ) ;
#4653 = CARTESIAN_POINT ( 'NONE',  ( 0.000000000000000000, 9.000000000000000000, 0.000000000000000000 ) ) ;
#4654 = EDGE_CURVE ( 'NONE', #11220, #1159, #8844, .T. ) ;
#4655 = DIRECTION ( 'NONE',  ( 0.000000000000000000, 0.000000000000000000, 1.000000000000000000 ) ) ;
#4656 = FACE_OUTER_BOUND ( 'NONE', #11464, .T. ) ;
#4657 = VECTOR ( 'NONE', #5345, 1000.000000000000000 ) ;
#4658 = DIRECTION ( 'NONE',  ( 0.000000000000000000, 1.000000000000000000, 0.000000000000000000 ) ) ;
#4659 = VECTOR ( 'NONE', #3912, 1000.000000000000000 ) ;
#4660 = CYLINDRICAL_SURFACE ( 'NONE', #2295, 12.08999999999737263 ) ;
#4661 = CARTESIAN_POINT ( 'NONE',  ( 5.170206418547656391, 3.000000000000000000, 13.27898586450067064 ) ) ;
#4662 = VERTEX_POINT ( 'NONE', #3681 ) ;
#4663 = ORIENTED_EDGE ( 'NONE', *, *, #11311, .T. ) ;
#4664 = ORIENTED_EDGE ( 'NONE', *, *, #1655, .T. ) ;
#4665 = ORIENTED_EDGE ( 'NONE', *, *, #1477, .F. ) ;
#4666 = CARTESIAN_POINT ( 'NONE',  ( 8.430890348300586368, 0.000000000000000000, -11.48836750521726913 ) ) ;
#4667 =( REPRESENTATION_RELATIONSHIP ('NONE','NONE', #3798, #6537 ) REPRESENTATION_RELATIONSHIP_WITH_TRANSFORMATION ( #3528 )SHAPE_REPRESENTATION_RELATIONSHIP( ) );
#4668 = B_SPLINE_CURVE_WITH_KNOTS ( 'NONE', 3,
 ( #1112, #5306, #8475, #4081 ),
 .UNSPECIFIED., .F., .F.,
 ( 4, 4 ),
 ( 0.000000000000000000, 0.8452273900860258760 ),
 .UNSPECIFIED. ) ;
#4669 = ORIENTED_EDGE ( 'NONE', *, *, #9184, .T. ) ;
#4670 = VECTOR ( 'NONE', #5919, 1000.000000000000000 ) ;
#4671 = AXIS2_PLACEMENT_3D ( 'NONE', #8011, #13332, #10077 ) ;
#4672 = AXIS2_PLACEMENT_3D ( 'NONE', #5521, #5595, #8750 ) ;
#4673 = DIRECTION ( 'NONE',  ( -0.000000000000000000, -1.000000000000000000, -0.000000000000000000 ) ) ;
#4674 = B_SPLINE_SURFACE_WITH_KNOTS ( 'NONE', 3, 1, ( 
 ( #7688, #2656 ),
 ( #1708, #6659 ),
 ( #2528, #5754 ),
 ( #667, #4861 ) ),
 .UNSPECIFIED., .F., .F., .F.,
 ( 4, 4 ),
 ( 2, 2 ),
 ( 0.000000000000000000, 0.8724294488011774540 ),
 ( 0.000000000000000000, 1.000000000000000000 ),
 .UNSPECIFIED. ) ;
#4675 = EDGE_CURVE ( 'NONE', #205, #2665, #11893, .T. ) ;
#4676 = LINE ( 'NONE', #5565, #9252 ) ;
#4677 = CARTESIAN_POINT ( 'NONE',  ( 31.00000000000000000, 0.000000000000000000, 1.499999998612421725 ) ) ;
#4678 = EDGE_CURVE ( 'NONE', #7143, #11405, #13444, .T. ) ;
#4679 = CARTESIAN_POINT ( 'NONE',  ( 12.00000000000000355, 2.749999999999990230, 10.00000000000000000 ) ) ;
#4680 = FACE_OUTER_BOUND ( 'NONE', #12737, .T. ) ;
#4681 = DIRECTION ( 'NONE',  ( 0.000000000000000000, 1.000000000000000000, 0.000000000000000000 ) ) ;
#4682 = ORIENTED_EDGE ( 'NONE', *, *, #12673, .T. ) ;
#4683 = CARTESIAN_POINT ( 'NONE',  ( -5.733772933379541747, 0.000000000000000000, -13.04554897075796482 ) ) ;
#4684 = CIRCLE ( 'NONE', #1164, 2.500000000000000444 ) ;
#4685 = EDGE_LOOP ( 'NONE', ( #1340, #1677, #9802, #10763 ) ) ;
#4686 = VERTEX_POINT ( 'NONE', #1639 ) ;
#4687 = CARTESIAN_POINT ( 'NONE',  ( -13.00394572736061605, 3.000000000000000000, 0.1835083749157108701 ) ) ;
#4688 = ORIENTED_EDGE ( 'NONE', *, *, #4160, .F. ) ;
#4689 = ORIENTED_EDGE ( 'NONE', *, *, #12348, .T. ) ;
#4690 = DIRECTION ( 'NONE',  ( 0.000000000000000000, -1.000000000000000000, 0.000000000000000000 ) ) ;
#4691 = AXIS2_PLACEMENT_3D ( 'NONE', #450, #4651, #12035 ) ;
#4692 = AXIS2_PLACEMENT_3D ( 'NONE', #8428, #12653, #3204 ) ;
#4693 = AXIS2_PLACEMENT_3D ( 'NONE', #338, #4529, #10672 ) ;
#4694 = CARTESIAN_POINT ( 'NONE',  ( 1.557181465540672161, 3.000000000000000000, -14.16466328168010591 ) ) ;
#4695 = CARTESIAN_POINT ( 'NONE',  ( -3.188443695493920593, 3.000000000000000000, -12.60833606734848189 ) ) ;
#4696 = CARTESIAN_POINT ( 'NONE',  ( -5.975392301194336397, 0.000000000000000000, -6.045220165289885372 ) ) ;
#4697 = DIRECTION ( 'NONE',  ( -0.000000000000000000, -1.000000000000000000, -0.000000000000000000 ) ) ;
#4698 = ORIENTED_EDGE ( 'NONE', *, *, #6502, .F. ) ;
#4699 = DIRECTION ( 'NONE',  ( 1.000000000000000000, -0.000000000000000000, 0.000000000000000000 ) ) ;
#4700 = ORIENTED_EDGE ( 'NONE', *, *, #8756, .F. ) ;
#4701 = AXIS2_PLACEMENT_3D ( 'NONE', #10365, #9260, #10441 ) ;
#4702 = ORIENTED_EDGE ( 'NONE', *, *, #9188, .T. ) ;
#4703 = AXIS2_PLACEMENT_3D ( 'NONE', #7037, #6758, #1674 ) ;
#4704 = B_SPLINE_CURVE_WITH_KNOTS ( 'NONE', 3,
 ( #6529, #4455, #11769, #7491 ),
 .UNSPECIFIED., .F., .F.,
 ( 4, 4 ),
 ( 0.000000000000000000, 0.8452273900860258760 ),
 .UNSPECIFIED. ) ;
#4705 = ORIENTED_EDGE ( 'NONE', *, *, #11547, .T. ) ;
#4706 = EDGE_CURVE ( 'NONE', #7580, #12590, #5752, .T. ) ;
#4707 = LINE ( 'NONE', #4778, #10156 ) ;
#4708 = CARTESIAN_POINT ( 'NONE',  ( -5.784789447945489549, 0.000000000000000000, 12.25836857253663581 ) ) ;
#4709 = CARTESIAN_POINT ( 'NONE',  ( -14.90895795148409420, 3.000000000000000000, 1.650143266773909101 ) ) ;
#4710 = DIRECTION ( 'NONE',  ( 0.000000000000000000, 0.000000000000000000, 1.000000000000000000 ) ) ;
#4711 = CARTESIAN_POINT ( 'NONE',  ( -21.21140389626389222, 3.000000000000000000, 12.49772878833445056 ) ) ;
#4712 = ITEM_DEFINED_TRANSFORMATION ( 'NONE', 'NONE', #354,  #10007 ) ;
#4713 = CIRCLE ( 'NONE', #11534, 8.500000000000000000 ) ;
#4714 = DIRECTION ( 'NONE',  ( 0.000000000000000000, 0.000000000000000000, 1.000000000000000000 ) ) ;
#4715 = AXIS2_PLACEMENT_3D ( 'NONE', #3549, #4658, #10864 ) ;
#4716 = DIRECTION ( 'NONE',  ( -0.000000000000000000, -1.000000000000000000, -0.000000000000000000 ) ) ;
#4717 = DIRECTION ( 'NONE',  ( 0.000000000000000000, 1.000000000000000000, 0.000000000000000000 ) ) ;
#4718 = LINE ( 'NONE', #10232, #1404 ) ;
#4719 = DIRECTION ( 'NONE',  ( 0.000000000000000000, 0.000000000000000000, 1.000000000000000000 ) ) ;
#4720 = ORIENTED_EDGE ( 'NONE', *, *, #7101, .T. ) ;
#4721 = ORIENTED_EDGE ( 'NONE', *, *, #6581, .F. ) ;
#4722 = AXIS2_PLACEMENT_3D ( 'NONE', #1070, #48, #12850 ) ;
#4723 = VECTOR ( 'NONE', #4771, 1000.000000000000000 ) ;
#4724 = ADVANCED_FACE ( 'NONE', ( #4589, #3480, #9683 ), #332, .F. ) ;
#4725 = EDGE_CURVE ( 'NONE', #13403, #9256, #52, .T. ) ;
#4726 = ORIENTED_EDGE ( 'NONE', *, *, #2547, .T. ) ;
#4727 = CARTESIAN_POINT ( 'NONE',  ( 30.73000000000000043, 3.000000000000000000, -5.500000000000003553 ) ) ;
#4728 = DIRECTION ( 'NONE',  ( 0.000000000000000000, 0.000000000000000000, -1.000000000000000000 ) ) ;
#4729 = ADVANCED_FACE ( 'NONE', ( #13066 ), #8646, .F. ) ;
#4730 = CARTESIAN_POINT ( 'NONE',  ( -5.250000000000000000, 3.000000000000000000, -29.44078293894052933 ) ) ;
#4731 = EDGE_CURVE ( 'NONE', #4943, #10892, #247, .T. ) ;
#4732 = LINE ( 'NONE', #2590, #10587 ) ;
#4733 = CARTESIAN_POINT ( 'NONE',  ( 5.958322434183388694, 9.000000000000000000, -6.062045345451230638 ) ) ;
#4734 = AXIS2_PLACEMENT_3D ( 'NONE', #2914, #8280, #3808 ) ;
#4735 = CARTESIAN_POINT ( 'NONE',  ( 46.02418392430381999, 0.000000000000000000, -15.41988256844266836 ) ) ;
#4736 = AXIS2_PLACEMENT_3D ( 'NONE', #1244, #3369, #10745 ) ;
#4737 = DIRECTION ( 'NONE',  ( -0.000000000000000000, -1.000000000000000000, -0.000000000000000000 ) ) ;
#4738 = DIRECTION ( 'NONE',  ( 1.000000000000000000, 0.000000000000000000, 1.224646799147353207E-16 ) ) ;
#4739 = ORIENTED_EDGE ( 'NONE', *, *, #13063, .T. ) ;
#4740 = EDGE_LOOP ( 'NONE', ( #7848, #2884, #7222, #3655 ) ) ;
#4741 = VERTEX_POINT ( 'NONE', #8774 ) ;
#4742 = CARTESIAN_POINT ( 'NONE',  ( 0.1834774187694905023, 0.000000000000000000, -13.00394734430440025 ) ) ;
#4743 = EDGE_CURVE ( 'NONE', #4566, #1383, #3546, .T. ) ;
#4744 = ORIENTED_EDGE ( 'NONE', *, *, #8055, .F. ) ;
#4745 = B_SPLINE_SURFACE_WITH_KNOTS ( 'NONE', 3, 1, ( 
 ( #801, #8345 ),
 ( #3945, #11530 ),
 ( #8147, #12514 ),
 ( #2095, #12379 ) ),
 .UNSPECIFIED., .F., .F., .F.,
 ( 4, 4 ),
 ( 2, 2 ),
 ( 0.000000000000000000, 0.5855695330273008592 ),
 ( 0.000000000000000000, 1.000000000000000000 ),
 .UNSPECIFIED. ) ;
#4746 = CARTESIAN_POINT ( 'NONE',  ( -13.49999999999999645, 3.000000000000000000, -7.049999999999998934 ) ) ;
#4747 = DIRECTION ( 'NONE',  ( -0.8254356770911585039, 7.100108776490246412E-29, -0.5644961850934520076 ) ) ;
#4748 = EDGE_CURVE ( 'NONE', #11943, #5243, #9050, .T. ) ;
#4749 = DIRECTION ( 'NONE',  ( -0.000000000000000000, -1.000000000000000000, 0.000000000000000000 ) ) ;
#4750 = FACE_OUTER_BOUND ( 'NONE', #46, .T. ) ;
#4751 = CARTESIAN_POINT ( 'NONE',  ( 9.375397774054407662, 0.000000000000000000, -11.70905276178460497 ) ) ;
#4752 = CARTESIAN_POINT ( 'NONE',  ( -8.352599575481690408, 3.000000000000000000, 28.00000000000000000 ) ) ;
#4753 = CYLINDRICAL_SURFACE ( 'NONE', #11116, 6.749999999999999112 ) ;
#4754 = ORIENTED_EDGE ( 'NONE', *, *, #8643, .F. ) ;
#4755 = FACE_OUTER_BOUND ( 'NONE', #4173, .T. ) ;
#4756 = DIRECTION ( 'NONE',  ( -0.000000000000000000, -1.000000000000000000, -0.000000000000000000 ) ) ;
#4757 = ORIENTED_EDGE ( 'NONE', *, *, #2446, .T. ) ;
#4758 = UNCERTAINTY_MEASURE_WITH_UNIT (LENGTH_MEASURE( 1.000000000000000082E-05 ), #13009, 'distance_accuracy_value', 'NONE');
#4759 = ORIENTED_EDGE ( 'NONE', *, *, #7932, .F. ) ;
#4760 = CARTESIAN_POINT ( 'NONE',  ( -8.430890348300559722, 3.000000000000000000, 11.48836750521728689 ) ) ;
#4761 = EDGE_CURVE ( 'NONE', #6683, #7859, #8731, .T. ) ;
#4762 = EDGE_CURVE ( 'NONE', #2558, #4834, #2454, .T. ) ;
#4764 = ORIENTED_EDGE ( 'NONE', *, *, #7541, .T. ) ;
#4763 = B_SPLINE_CURVE_WITH_KNOTS ( 'NONE', 3,
 ( #7998, #11105, #6823, #7854 ),
 .UNSPECIFIED., .F., .F.,
 ( 4, 4 ),
 ( 0.1547128134717859205, 1.000000000000000000 ),
 .UNSPECIFIED. ) ;
#4765 = VERTEX_POINT ( 'NONE', #9135 ) ;
#4766 = FACE_OUTER_BOUND ( 'NONE', #4967, .T. ) ;
#4767 = CARTESIAN_POINT ( 'NONE',  ( -8.795158114916672432, 0.000000000000000000, -9.573149624528774382 ) ) ;
#4768 = FILL_AREA_STYLE_COLOUR ( '', #7484 ) ;
#4769 = CYLINDRICAL_SURFACE ( 'NONE', #5150, 6.750000000000000888 ) ;
#4770 = CARTESIAN_POINT ( 'NONE',  ( 2.568302020731520141, 3.000000000000000000, 12.56087513340552420 ) ) ;
#4771 = DIRECTION ( 'NONE',  ( -0.000000000000000000, -1.000000000000000000, -0.000000000000000000 ) ) ;
#4772 = EDGE_LOOP ( 'NONE', ( #4599, #13109, #12858, #8092 ) ) ;
#4773 = LINE ( 'NONE', #8957, #4900 ) ;
#4774 = ORIENTED_EDGE ( 'NONE', *, *, #1059, .F. ) ;
#4775 = EDGE_LOOP ( 'NONE', ( #251, #7512, #4156, #10074 ) ) ;
#4776 = EDGE_CURVE ( 'NONE', #1924, #116, #11473, .T. ) ;
#4777 = ORIENTED_EDGE ( 'NONE', *, *, #11140, .T. ) ;
#4778 = CARTESIAN_POINT ( 'NONE',  ( 10.00000000000002309, 8.000000000000007105, 10.00000000000000178 ) ) ;
#4779 = DIRECTION ( 'NONE',  ( 0.000000000000000000, 0.000000000000000000, 1.000000000000000000 ) ) ;
#4780 = CARTESIAN_POINT ( 'NONE',  ( -7.494008246337227952, 3.000000000000000000, -11.63517940784355886 ) ) ;
#4781 = CARTESIAN_POINT ( 'NONE',  ( -13.04554897075796127, 3.000000000000000000, 5.733772933379547077 ) ) ;
#4782 = CARTESIAN_POINT ( 'NONE',  ( 2.719999999999997087, 0.000000000000000000, -4.500000000000000888 ) ) ;
#4783 = CARTESIAN_POINT ( 'NONE',  ( 5.452638258930520010, 0.000000000000000000, -13.97385902380752754 ) ) ;
#4784 = LINE ( 'NONE', #4846, #3760 ) ;
#4785 = CARTESIAN_POINT ( 'NONE',  ( 29.02231267299996986, 0.000000000000000000, -1.321950885510182250 ) ) ;
#4786 = CIRCLE ( 'NONE', #12285, 8.499999999999996447 ) ;
#4787 = DIRECTION ( 'NONE',  ( 0.000000000000000000, 1.000000000000000000, -0.000000000000000000 ) ) ;
#4788 = ORIENTED_EDGE ( 'NONE', *, *, #3885, .T. ) ;
#4789 = EDGE_CURVE ( 'NONE', #13316, #11616, #4859, .T. ) ;
#4790 = ORIENTED_EDGE ( 'NONE', *, *, #2600, .T. ) ;
#4791 = ORIENTED_EDGE ( 'NONE', *, *, #1773, .T. ) ;
#4792 = CARTESIAN_POINT ( 'NONE',  ( 13.04554897075798081, 0.000000000000000000, -5.733772933379503556 ) ) ;
#4793 = DIRECTION ( 'NONE',  ( -3.469446951953614189E-15, -1.000000000000000000, 0.000000000000000000 ) ) ;
#4794 = LINE ( 'NONE', #8980, #13490 ) ;
#4795 = CARTESIAN_POINT ( 'NONE',  ( 0.000000000000000000, 0.000000000000000000, 0.000000000000000000 ) ) ;
#4796 = FACE_OUTER_BOUND ( 'NONE', #11403, .T. ) ;
#4797 = CARTESIAN_POINT ( 'NONE',  ( 31.00000000000000000, 3.000000000000000000, -1.500000000759764029 ) ) ;
#4798 = DIRECTION ( 'NONE',  ( 0.000000000000000000, 1.000000000000000000, 0.000000000000000000 ) ) ;
#4799 = EDGE_CURVE ( 'NONE', #8041, #7779, #7503, .T. ) ;
#4800 = DIRECTION ( 'NONE',  ( -0.000000000000000000, -1.000000000000000000, -0.000000000000000000 ) ) ;
#4801 = VERTEX_POINT ( 'NONE', #7150 ) ;
#4802 = ORIENTED_EDGE ( 'NONE', *, *, #9313, .F. ) ;
#4803 = VERTEX_POINT ( 'NONE', #8161 ) ;
#4804 = DIRECTION ( 'NONE',  ( 0.000000000000000000, 1.000000000000000000, 0.000000000000000000 ) ) ;
#4805 = ORIENTED_EDGE ( 'NONE', *, *, #9624, .F. ) ;
#4806 = CARTESIAN_POINT ( 'NONE',  ( 12.48730470360076161, 3.000000000000000000, -6.329867395090054139 ) ) ;
#4807 = CARTESIAN_POINT ( 'NONE',  ( 23.42696780347059970, 31.33135765298363040, 14.10964106096158233 ) ) ;
#4808 = CARTESIAN_POINT ( 'NONE',  ( 7.146769547044127258, 9.000000000000000000, -1.771712133291270863 ) ) ;
#4809 = CARTESIAN_POINT ( 'NONE',  ( -1.161309641800940540, -1.694065894508600678E-18, -7.856984441350959969 ) ) ;
#4810 = CARTESIAN_POINT ( 'NONE',  ( 29.39270799701850123, 0.000000000000000000, -0.3930766723116408401 ) ) ;
#4811 = EDGE_CURVE ( 'NONE', #9688, #692, #4936, .T. ) ;
#4812 = LINE ( 'NONE', #5912, #717 ) ;
#4813 = CYLINDRICAL_SURFACE ( 'NONE', #2103, 12.00000000000000000 ) ;
#4814 = ORIENTED_EDGE ( 'NONE', *, *, #11409, .T. ) ;
#4815 = PLANE ( 'NONE',  #12406 ) ;
#4816 = ORIENTED_EDGE ( 'NONE', *, *, #427, .F. ) ;
#4817 = EDGE_CURVE ( 'NONE', #6179, #12863, #8590, .T. ) ;
#4818 = ORIENTED_EDGE ( 'NONE', *, *, #5906, .T. ) ;
#4819 = DIRECTION ( 'NONE',  ( -0.000000000000000000, -1.000000000000000000, 0.000000000000000000 ) ) ;
#4820 = ADVANCED_FACE ( 'NONE', ( #3831, #3008, #13350, #6107, #13408 ), #7214, .T. ) ;
#4821 = ORIENTED_EDGE ( 'NONE', *, *, #8249, .F. ) ;
#4822 = FACE_OUTER_BOUND ( 'NONE', #8349, .T. ) ;
#4823 = ORIENTED_EDGE ( 'NONE', *, *, #9444, .F. ) ;
#4824 = DIRECTION ( 'NONE',  ( -0.000000000000000000, -1.000000000000000000, -0.000000000000000000 ) ) ;
#4825 = CARTESIAN_POINT ( 'NONE',  ( -18.21140389626389577, 3.000000000000000000, -14.83930531255816376 ) ) ;
#4826 = CARTESIAN_POINT ( 'NONE',  ( 0.7901945867173618687, 0.000000000000000000, 12.78643498603817541 ) ) ;
#4827 = CARTESIAN_POINT ( 'NONE',  ( -12.07793442604883971, 0.000000000000000000, 0.5400000000008015055 ) ) ;
#4828 = FACE_OUTER_BOUND ( 'NONE', #7514, .T. ) ;
#4829 = VECTOR ( 'NONE', #9766, 1000.000000000000000 ) ;
#4830 = DIRECTION ( 'NONE',  ( -0.000000000000000000, -1.000000000000000000, 0.000000000000000000 ) ) ;
#4831 = VERTEX_POINT ( 'NONE', #12320 ) ;
#4832 = DIRECTION ( 'NONE',  ( 0.000000000000000000, 0.000000000000000000, 1.000000000000000000 ) ) ;
#4833 = ORIENTED_EDGE ( 'NONE', *, *, #13209, .F. ) ;
#4834 = VERTEX_POINT ( 'NONE', #4037 ) ;
#4835 = CARTESIAN_POINT ( 'NONE',  ( 8.373678438139048552, 0.000000000000000000, 1.459968977288628178 ) ) ;
#4836 = ORIENTED_EDGE ( 'NONE', *, *, #9198, .F. ) ;
#4837 = TOROIDAL_SURFACE ( 'NONE', #5487, 3.100000000000000977, 0.1000000000000000056 ) ;
#4838 = AXIS2_PLACEMENT_3D ( 'NONE', #921, #9323, #2090 ) ;
#4839 = DIRECTION ( 'NONE',  ( 0.000000000000000000, 1.000000000000000000, -0.000000000000000000 ) ) ;
#4840 = FACE_OUTER_BOUND ( 'NONE', #2536, .T. ) ;
#4841 = CARTESIAN_POINT ( 'NONE',  ( 20.03271148078819408, 3.000000000000000000, -5.075121771833452478 ) ) ;
#4842 = CARTESIAN_POINT ( 'NONE',  ( 0.000000000000000000, 3.000000000000000000, 0.000000000000000000 ) ) ;
#4843 = DIRECTION ( 'NONE',  ( 0.000000000000000000, 1.000000000000000000, 0.000000000000000000 ) ) ;
#4844 = EDGE_CURVE ( 'NONE', #12757, #3458, #742, .T. ) ;
#4845 = FACE_OUTER_BOUND ( 'NONE', #7120, .T. ) ;
#4846 = CARTESIAN_POINT ( 'NONE',  ( 0.000000000000000000, 1.000000000000000000, -2.500000000000000444 ) ) ;
#4847 = ADVANCED_FACE ( 'NONE', ( #12468 ), #4837, .T. ) ;
#4848 = CARTESIAN_POINT ( 'NONE',  ( 11.13895890373327724, 0.000000000000000000, -7.723663868796764476 ) ) ;
#4849 = CARTESIAN_POINT ( 'NONE',  ( -4.072642252455976219, 0.000000000000000000, -12.14623037080101398 ) ) ;
#4850 =( REPRESENTATION_RELATIONSHIP ('NONE','NONE', #3798, #2323 ) REPRESENTATION_RELATIONSHIP_WITH_TRANSFORMATION ( #10976 )SHAPE_REPRESENTATION_RELATIONSHIP( ) );
#4851 = CIRCLE ( 'NONE', #6608, 8.499999999999996447 ) ;
#4852 = ORIENTED_EDGE ( 'NONE', *, *, #12742, .F. ) ;
#4853 = ORIENTED_EDGE ( 'NONE', *, *, #13161, .T. ) ;
#4854 = ORIENTED_EDGE ( 'NONE', *, *, #10783, .T. ) ;
#4855 = DIRECTION ( 'NONE',  ( -0.000000000000000000, -1.000000000000000000, -0.000000000000000000 ) ) ;
#4856 = CIRCLE ( 'NONE', #10359, 1.499999999686092877 ) ;
#4857 = CIRCLE ( 'NONE', #6832, 12.08999999999737440 ) ;
#4858 = DIRECTION ( 'NONE',  ( 0.000000000000000000, 0.000000000000000000, 1.000000000000000000 ) ) ;
#4859 = LINE ( 'NONE', #6935, #6806 ) ;
#4860 = FACE_OUTER_BOUND ( 'NONE', #2803, .T. ) ;
#4861 = CARTESIAN_POINT ( 'NONE',  ( 7.248474140376191421, 0.000000000000000000, 4.439552076088042476 ) ) ;
#4862 = LINE ( 'NONE', #13278, #2734 ) ;
#4863 = CARTESIAN_POINT ( 'NONE',  ( 8.504652361247167391, 0.000000000000000000, 9.593885948927674434 ) ) ;
#4864 = ORIENTED_EDGE ( 'NONE', *, *, #1543, .T. ) ;
#4865 = AXIS2_PLACEMENT_3D ( 'NONE', #4513, #1273, #11817 ) ;
#4866 = VERTEX_POINT ( 'NONE', #12255 ) ;
#4867 = ORIENTED_EDGE ( 'NONE', *, *, #9280, .T. ) ;
#4868 = CARTESIAN_POINT ( 'NONE',  ( -2.161962830978702677, 0.000000000000000000, 14.08504230442587435 ) ) ;
#4869 = ORIENTED_EDGE ( 'NONE', *, *, #936, .T. ) ;
#4870 = EDGE_CURVE ( 'NONE', #8226, #1004, #10368, .T. ) ;
#4871 = DIRECTION ( 'NONE',  ( 0.000000000000000000, 0.000000000000000000, -1.000000000000000000 ) ) ;
#4872 = DIRECTION ( 'NONE',  ( 0.5494223406819142008, 1.100657519464115479E-21, -0.8355447872852816982 ) ) ;
#4873 = AXIS2_PLACEMENT_3D ( 'NONE', #840, #1042, #13447 ) ;
#4874 = LINE ( 'NONE', #7164, #8151 ) ;
#4875 = CARTESIAN_POINT ( 'NONE',  ( -11.48836750521723893, 3.000000000000000000, 8.430890348300625448 ) ) ;
#4876 = DIRECTION ( 'NONE',  ( 0.000000000000000000, -0.000000000000000000, 1.000000000000000000 ) ) ;
#4877 = CARTESIAN_POINT ( 'NONE',  ( -8.914835885878282795, 3.000000000000000000, -11.11702303352191556 ) ) ;
#4878 = CARTESIAN_POINT ( 'NONE',  ( 0.000000000000000000, 9.000000000000000000, 0.000000000000000000 ) ) ;
#4879 = ORIENTED_EDGE ( 'NONE', *, *, #6391, .F. ) ;
#4880 = SURFACE_STYLE_FILL_AREA ( #6805 ) ;
#4881 = EDGE_LOOP ( 'NONE', ( #8205, #2627, #1872, #4168 ) ) ;
#4882 = VECTOR ( 'NONE', #11621, 1000.000000000000000 ) ;
#4883 = ORIENTED_EDGE ( 'NONE', *, *, #3070, .T. ) ;
#4884 = CARTESIAN_POINT ( 'NONE',  ( 6.506507307819716424, 0.000000000000000000, -10.18987059060247269 ) ) ;
#4885 = AXIS2_PLACEMENT_3D ( 'NONE', #13253, #12085, #12231 ) ;
#4886 = AXIS2_PLACEMENT_3D ( 'NONE', #7738, #10917, #11752 ) ;
#4887 = EDGE_LOOP ( 'NONE', ( #6159, #11460, #10997, #2414 ) ) ;
#4888 = CARTESIAN_POINT ( 'NONE',  ( 3.542895259386137585, 0.000000000000000000, -12.51336047125611017 ) ) ;
#4889 = EDGE_CURVE ( 'NONE', #2066, #688, #8351, .T. ) ;
#4890 = EDGE_LOOP ( 'NONE', ( #4546, #4221, #8890, #7287 ) ) ;
#4891 = EDGE_CURVE ( 'NONE', #846, #11264, #9914, .T. ) ;
#4892 = DIRECTION ( 'NONE',  ( -0.000000000000000000, -1.000000000000000000, -0.000000000000000000 ) ) ;
#4893 = CARTESIAN_POINT ( 'NONE',  ( 7.248474140376192310, 9.000000000000000000, 4.439552076088041588 ) ) ;
#4894 = CARTESIAN_POINT ( 'NONE',  ( 20.00000000000001421, 5.999999999999972466, -5.204170427930418128E-15 ) ) ;
#4895 = AXIS2_PLACEMENT_3D ( 'NONE', #3504, #1459, #9910 ) ;
#4896 = ADVANCED_FACE ( 'NONE', ( #7005 ), #11348, .T. ) ;
#4897 = CARTESIAN_POINT ( 'NONE',  ( -6.558450276537426404, 9.000000000000000000, -1.596630818375423866 ) ) ;
#4898 = CIRCLE ( 'NONE', #2046, 2.000000000000000444 ) ;
#4899 = EDGE_CURVE ( 'NONE', #816, #11204, #10162, .T. ) ;
#4900 = VECTOR ( 'NONE', #3721, 1000.000000000000000 ) ;
#4901 = CARTESIAN_POINT ( 'NONE',  ( 2.604531154829233586, 3.000000000000000000, 11.80612203322752585 ) ) ;
#4902 = CYLINDRICAL_SURFACE ( 'NONE', #11110, 0.7500000000000024425 ) ;
#4903 = ORIENTED_EDGE ( 'NONE', *, *, #613, .F. ) ;
#4904 = CYLINDRICAL_SURFACE ( 'NONE', #1380, 5.486375544325371223 ) ;
#4905 = B_SPLINE_CURVE_WITH_KNOTS ( 'NONE', 3,
 ( #4012, #10286, #10222, #5943 ),
 .UNSPECIFIED., .F., .F.,
 ( 4, 4 ),
 ( 0.1547128134717859205, 1.000000000000000000 ),
 .UNSPECIFIED. ) ;
#4906 = ORIENTED_EDGE ( 'NONE', *, *, #2054, .T. ) ;
#4907 = EDGE_LOOP ( 'NONE', ( #7267, #10315, #4739, #12364 ) ) ;
#4908 = CARTESIAN_POINT ( 'NONE',  ( -1.557181465540221188, 3.000000000000000000, 14.16466328168015743 ) ) ;
#4909 = ORIENTED_EDGE ( 'NONE', *, *, #7920, .F. ) ;
#4910 = VECTOR ( 'NONE', #6198, 1000.000000000000000 ) ;
#4911 = AXIS2_PLACEMENT_3D ( 'NONE', #11918, #1108, #8531 ) ;
#4912 = EDGE_CURVE ( 'NONE', #1515, #1280, #7956, .T. ) ;
#4913 = CARTESIAN_POINT ( 'NONE',  ( 8.158651161643900807, 0.000000000000000000, 8.922136023539609440 ) ) ;
#4914 = CARTESIAN_POINT ( 'NONE',  ( -8.883544964652065445, 3.000000000000000000, -12.08646469655229438 ) ) ;
#4915 = CARTESIAN_POINT ( 'NONE',  ( -2.830255545554292151, 3.000000000000000000, -12.68816982652971959 ) ) ;
#4916 = CARTESIAN_POINT ( 'NONE',  ( -4.679611352264966051, 0.000000000000000000, -6.417326716594978997 ) ) ;
#4917 = DIRECTION ( 'NONE',  ( 0.000000000000000000, 1.000000000000000000, 0.000000000000000000 ) ) ;
#4918 = ADVANCED_FACE ( 'NONE', ( #1706 ), #663, .T. ) ;
#4919 = CARTESIAN_POINT ( 'NONE',  ( -4.190859029938718727, -1.694065894508600678E-18, -6.054087828318142073 ) ) ;
#4920 = CARTESIAN_POINT ( 'NONE',  ( -10.18979803820068675, 3.000000000000000000, 6.506620931068438196 ) ) ;
#4921 = AXIS2_PLACEMENT_3D ( 'NONE', #2760, #6966, #11162 ) ;
#4922 = DIRECTION ( 'NONE',  ( 1.224646799147353454E-16, 0.000000000000000000, -1.000000000000000000 ) ) ;
#4923 = FACE_OUTER_BOUND ( 'NONE', #7027, .T. ) ;
#4924 = AXIS2_PLACEMENT_3D ( 'NONE', #3943, #3736, #5882 ) ;
#4925 = CIRCLE ( 'NONE', #2936, 1.500000000000000222 ) ;
#4926 = ORIENTED_EDGE ( 'NONE', *, *, #362, .F. ) ;
#4927 = VERTEX_POINT ( 'NONE', #12587 ) ;
#4928 = ORIENTED_EDGE ( 'NONE', *, *, #11148, .F. ) ;
#4929 = EDGE_CURVE ( 'NONE', #3134, #12940, #6596, .T. ) ;
#4930 = EDGE_CURVE ( 'NONE', #9908, #748, #2417, .T. ) ;
#4931 = VERTEX_POINT ( 'NONE', #7411 ) ;
#4932 = DIRECTION ( 'NONE',  ( 0.000000000000000000, 1.000000000000000000, -0.000000000000000000 ) ) ;
#4933 = VECTOR ( 'NONE', #7075, 1000.000000000000000 ) ;
#4934 = DIRECTION ( 'NONE',  ( -0.000000000000000000, -1.000000000000000000, -0.000000000000000000 ) ) ;
#4935 = APPLICATION_CONTEXT ( 'automotive_design' ) ;
#4936 = LINE ( 'NONE', #9055, #10113 ) ;
#4937 = DIRECTION ( 'NONE',  ( 1.000000000000000000, -0.000000000000000000, 0.000000000000000000 ) ) ;
#4938 = B_SPLINE_CURVE_WITH_KNOTS ( 'NONE', 3,
 ( #5666, #9863, #12023, #10972 ),
 .UNSPECIFIED., .F., .F.,
 ( 4, 4 ),
 ( 0.2280192144657617603, 0.8452273900860258760 ),
 .UNSPECIFIED. ) ;
#4939 = LINE ( 'NONE', #3010, #11756 ) ;
#4940 =( GEOMETRIC_REPRESENTATION_CONTEXT ( 3 ) GLOBAL_UNCERTAINTY_ASSIGNED_CONTEXT ( ( #6809 ) ) GLOBAL_UNIT_ASSIGNED_CONTEXT ( ( #10648, #5401, #123 ) ) REPRESENTATION_CONTEXT ( 'NONE', 'WORKASPACE' ) );
#4941 = CARTESIAN_POINT ( 'NONE',  ( -0.7702044561450404059, 3.000000000000000000, 12.79759916868914793 ) ) ;
#4942 = CIRCLE ( 'NONE', #10662, 0.1000000000000001166 ) ;
#4943 = VERTEX_POINT ( 'NONE', #2108 ) ;
#4944 = ORIENTED_EDGE ( 'NONE', *, *, #2697, .F. ) ;
#4945 = TOROIDAL_SURFACE ( 'NONE', #13308, 3.100000000000000977, 0.1000000000000000056 ) ;
#4946 = ORIENTED_EDGE ( 'NONE', *, *, #7922, .T. ) ;
#4947 = DIRECTION ( 'NONE',  ( 0.000000000000000000, 1.000000000000000000, -0.000000000000000000 ) ) ;
#4948 = VERTEX_POINT ( 'NONE', #4370 ) ;
#4949 = FACE_OUTER_BOUND ( 'NONE', #8473, .T. ) ;
#4950 = VECTOR ( 'NONE', #30, 1000.000000000000000 ) ;
#4951 = DIRECTION ( 'NONE',  ( 1.000000000000000000, 0.000000000000000000, 0.000000000000000000 ) ) ;
#4952 = VECTOR ( 'NONE', #13448, 1000.000000000000000 ) ;
#4953 = DIRECTION ( 'NONE',  ( 0.000000000000000000, 0.000000000000000000, 1.000000000000000000 ) ) ;
#4954 = CARTESIAN_POINT ( 'NONE',  ( -0.5501230721523990841, 3.000000000000000000, -12.98835496148299384 ) ) ;
#4955 = CARTESIAN_POINT ( 'NONE',  ( 5.797378255456016483, 0.000000000000000000, 12.25282671965375592 ) ) ;
#4956 = CARTESIAN_POINT ( 'NONE',  ( 0.000000000000000000, 9.000000000000000000, 0.000000000000000000 ) ) ;
#4957 = CARTESIAN_POINT ( 'NONE',  ( 2.458659560121116527, 9.000000000000000000, -8.136645080586040635 ) ) ;
#4958 = ORIENTED_EDGE ( 'NONE', *, *, #1537, .T. ) ;
#4959 = CARTESIAN_POINT ( 'NONE',  ( 10.00000000000001243, 5.250000000000007105, -2.602085213965208275E-15 ) ) ;
#4960 = ORIENTED_EDGE ( 'NONE', *, *, #6068, .T. ) ;
#4961 = ADVANCED_FACE ( 'NONE', ( #8361 ), #12760, .T. ) ;
#4962 = ORIENTED_EDGE ( 'NONE', *, *, #7501, .T. ) ;
#4963 = VERTEX_POINT ( 'NONE', #4165 ) ;
#4964 = VECTOR ( 'NONE', #6460, 1000.000000000000000 ) ;
#4965 = CARTESIAN_POINT ( 'NONE',  ( 9.375397774054407662, 3.000000000000000000, -11.70905276178460497 ) ) ;
#4966 = ORIENTED_EDGE ( 'NONE', *, *, #565, .T. ) ;
#4967 = EDGE_LOOP ( 'NONE', ( #4663, #7480, #1439, #12659 ) ) ;
#4968 = CARTESIAN_POINT ( 'NONE',  ( 0.000000000000000000, 2.900000000000000355, 0.000000000000000000 ) ) ;
#4969 = CARTESIAN_POINT ( 'NONE',  ( -13.52637830886139092, 0.000000000000000000, 2.928250210355532790 ) ) ;
#4970 =( LENGTH_UNIT ( ) NAMED_UNIT ( * ) SI_UNIT ( .MILLI., .METRE. ) );
#4971 = CARTESIAN_POINT ( 'NONE',  ( -9.299128225235689271, 3.000000000000000000, -10.25006213149501555 ) ) ;
#4972 = DIRECTION ( 'NONE',  ( -0.000000000000000000, -1.000000000000000000, -0.000000000000000000 ) ) ;
#4973 = CARTESIAN_POINT ( 'NONE',  ( -1.557181465540760534, 3.000000000000000000, -14.16466328168009703 ) ) ;
#4974 = ORIENTED_EDGE ( 'NONE', *, *, #8509, .F. ) ;
#4975 = CARTESIAN_POINT ( 'NONE',  ( -2.604399508763951321, 3.000000000000000000, 11.80615107470197422 ) ) ;
#4976 = EDGE_CURVE ( 'NONE', #8568, #4097, #1975, .T. ) ;
#4977 = EDGE_LOOP ( 'NONE', ( #5379, #5321, #11576, #10737 ) ) ;
#4978 = ADVANCED_FACE ( 'NONE', ( #6367 ), #5210, .T. ) ;
#4979 = ORIENTED_EDGE ( 'NONE', *, *, #2022, .F. ) ;
#4980 = CARTESIAN_POINT ( 'NONE',  ( -3.835481108877868195, 1.734723475976807094E-15, 5.554420281491219136 ) ) ;
#4981 = EDGE_LOOP ( 'NONE', ( #697, #12186, #7245, #12343 ) ) ;
#4982 = ADVANCED_FACE ( 'NONE', ( #1139 ), #2157, .F. ) ;
#4983 = CARTESIAN_POINT ( 'NONE',  ( 2.161962830978677363, 3.000000000000000000, 14.08504230442587613 ) ) ;
#4984 = CARTESIAN_POINT ( 'NONE',  ( 12.08646469655232636, 3.000000000000000000, -8.883544964652022813 ) ) ;
#4985 = FACE_OUTER_BOUND ( 'NONE', #4124, .T. ) ;
#4986 = LINE ( 'NONE', #9179, #3727 ) ;
#4987 = CARTESIAN_POINT ( 'NONE',  ( 0.000000000000000000, 0.000000000000000000, 0.000000000000000000 ) ) ;
#4988 = CARTESIAN_POINT ( 'NONE',  ( 31.00000000000000000, 0.09999999999999982514, 0.000000000000000000 ) ) ;
#4989 = LINE ( 'NONE', #3880, #13457 ) ;
#4990 = CARTESIAN_POINT ( 'NONE',  ( 53.04054522416362261, 3.000000000000000000, -3.611077387296437013 ) ) ;
#4991 = DIRECTION ( 'NONE',  ( 0.000000000000000000, 0.000000000000000000, -1.000000000000000000 ) ) ;
#4992 = DIRECTION ( 'NONE',  ( -9.145772869372436484E-17, 0.000000000000000000, -1.000000000000000000 ) ) ;
#4993 = EDGE_CURVE ( 'NONE', #1111, #11851, #7265, .T. ) ;
#4994 = ORIENTED_EDGE ( 'NONE', *, *, #12268, .F. ) ;
#4995 = ORIENTED_EDGE ( 'NONE', *, *, #7755, .F. ) ;
#4996 = VERTEX_POINT ( 'NONE', #1072 ) ;
#4997 = EDGE_CURVE ( 'NONE', #655, #10050, #8562, .T. ) ;
#4998 = EDGE_CURVE ( 'NONE', #12645, #9873, #3322, .T. ) ;
#4999 = ORIENTED_EDGE ( 'NONE', *, *, #12559, .F. ) ;
#5000 = DIRECTION ( 'NONE',  ( 0.000000000000000000, 1.000000000000000000, 0.000000000000000000 ) ) ;
#5001 = CARTESIAN_POINT ( 'NONE',  ( 28.54655175640005282, 2.900000000000000355, 2.353846153846155254 ) ) ;
#5002 = CARTESIAN_POINT ( 'NONE',  ( 19.60942157306000766, 0.000000000000000000, 14.05941790610251374 ) ) ;
#5003 = CARTESIAN_POINT ( 'NONE',  ( 0.000000000000000000, 3.000000000000000000, 0.000000000000000000 ) ) ;
#5004 = DIRECTION ( 'NONE',  ( -0.000000000000000000, -1.000000000000000000, -0.000000000000000000 ) ) ;
#5005 = EDGE_CURVE ( 'NONE', #13346, #11587, #3983, .T. ) ;
#5006 = CARTESIAN_POINT ( 'NONE',  ( -12.79759916868914615, 0.000000000000000000, -0.7702044561450367421 ) ) ;
#5007 = EDGE_CURVE ( 'NONE', #9584, #9307, #5788, .T. ) ;
#5008 = PLANE ( 'NONE',  #7556 ) ;
#5009 = ORIENTED_EDGE ( 'NONE', *, *, #12723, .F. ) ;
#5010 = CYLINDRICAL_SURFACE ( 'NONE', #1811, 5.499999999999996447 ) ;
#5011 = CARTESIAN_POINT ( 'NONE',  ( 10.72979803820132005, 0.000000000000000000, 5.571313494980133285 ) ) ;
#5012 = EDGE_LOOP ( 'NONE', ( #10920, #8741 ) ) ;
#5013 = CARTESIAN_POINT ( 'NONE',  ( -2.481593227817850966, 0.000000000000000000, -8.129679886173169834 ) ) ;
#5014 = DIRECTION ( 'NONE',  ( -0.7526020642202010391, -6.057154494016760914E-23, 0.6584756130119723272 ) ) ;
#5015 = CARTESIAN_POINT ( 'NONE',  ( -11.80615107470197778, 0.000000000000000000, -2.604399508763947768 ) ) ;
#5016 = DIRECTION ( 'NONE',  ( -0.000000000000000000, -1.000000000000000000, -0.000000000000000000 ) ) ;
#5017 = CARTESIAN_POINT ( 'NONE',  ( -14.90895795148411374, 3.000000000000000000, -1.650143266773683726 ) ) ;
#5018 = CARTESIAN_POINT ( 'NONE',  ( 2.830255545554135832, 3.000000000000000000, -12.68816982652952596 ) ) ;
#5019 = EDGE_CURVE ( 'NONE', #13428, #10501, #4308, .T. ) ;
#5020 = LINE ( 'NONE', #3984, #6939 ) ;
#5021 = EDGE_CURVE ( 'NONE', #12534, #288, #2234, .T. ) ;
#5022 = ORIENTED_EDGE ( 'NONE', *, *, #3909, .T. ) ;
#5023 = CARTESIAN_POINT ( 'NONE',  ( 2.414978278956333213, 0.000000000000000000, -13.33788847341978645 ) ) ;
#5024 = EDGE_LOOP ( 'NONE', ( #1553, #4601, #1533, #12899 ) ) ;
#5025 = ORIENTED_EDGE ( 'NONE', *, *, #10865, .T. ) ;
#5026 = LINE ( 'NONE', #12206, #13029 ) ;
#5027 = VERTEX_POINT ( 'NONE', #3330 ) ;
#5028 = CARTESIAN_POINT ( 'NONE',  ( -18.21140389626389577, 0.000000000000000000, -14.83930531255816376 ) ) ;
#5029 = FACE_OUTER_BOUND ( 'NONE', #7031, .T. ) ;
#5030 = SURFACE_STYLE_FILL_AREA ( #7180 ) ;
#5031 = EDGE_CURVE ( 'NONE', #4317, #12707, #940, .T. ) ;
#5032 = DIRECTION ( 'NONE',  ( -0.000000000000000000, -1.000000000000000000, -0.000000000000000000 ) ) ;
#5033 = CARTESIAN_POINT ( 'NONE',  ( 0.000000000000000000, 0.000000000000000000, 0.000000000000000000 ) ) ;
#5034 = DIRECTION ( 'NONE',  ( -0.000000000000000000, -1.000000000000000000, -0.000000000000000000 ) ) ;
#5035 = ORIENTED_EDGE ( 'NONE', *, *, #10540, .F. ) ;
#5036 = DIRECTION ( 'NONE',  ( -0.000000000000000000, -1.000000000000000000, -0.000000000000000000 ) ) ;
#5037 = ORIENTED_EDGE ( 'NONE', *, *, #5308, .F. ) ;
#5038 = ORIENTED_EDGE ( 'NONE', *, *, #7769, .F. ) ;
#5039 = CARTESIAN_POINT ( 'NONE',  ( 7.499999999999999112, 0.000000000000000000, -1.499999999999997780 ) ) ;
#5040 = ORIENTED_EDGE ( 'NONE', *, *, #3148, .T. ) ;
#5041 = DIRECTION ( 'NONE',  ( -0.000000000000000000, -1.000000000000000000, -0.000000000000000000 ) ) ;
#5042 = CARTESIAN_POINT ( 'NONE',  ( -8.222660081691577361, 3.000000000000000000, -5.549999999999999822 ) ) ;
#5043 = CARTESIAN_POINT ( 'NONE',  ( -11.90209577080766046, 0.000000000000000000, -8.180229652970757215 ) ) ;
#5044 = CARTESIAN_POINT ( 'NONE',  ( 2.264806262022877714, 3.000000000000000000, -14.82803603298501471 ) ) ;
#5045 = CIRCLE ( 'NONE', #4602, 12.08999999999737440 ) ;
#5046 = EDGE_CURVE ( 'NONE', #1608, #10985, #4473, .T. ) ;
#5047 = CARTESIAN_POINT ( 'NONE',  ( -5.733772933379472470, 0.000000000000000000, 13.04554897075799502 ) ) ;
#5048 = CONTEXT_DEPENDENT_SHAPE_REPRESENTATION ( #13388, #8866 ) ;
#5049 = CARTESIAN_POINT ( 'NONE',  ( -14.90895795148411374, 0.000000000000000000, -1.650143266773683726 ) ) ;
#5050 = CARTESIAN_POINT ( 'NONE',  ( -0.5501230721523990841, 3.000000000000000000, -12.98835496148299384 ) ) ;
#5051 = LINE ( 'NONE', #11602, #11257 ) ;
#5052 = ORIENTED_EDGE ( 'NONE', *, *, #4467, .F. ) ;
#5053 = DIRECTION ( 'NONE',  ( 0.000000000000000000, 0.000000000000000000, -1.000000000000000000 ) ) ;
#5054 = ORIENTED_EDGE ( 'NONE', *, *, #6505, .T. ) ;
#5055 = EDGE_LOOP ( 'NONE', ( #8581, #9745, #7912, #12369 ) ) ;
#5056 = VECTOR ( 'NONE', #8300, 1000.000000000000000 ) ;
#5057 = AXIS2_PLACEMENT_3D ( 'NONE', #9448, #170, #12834 ) ;
#5058 = ORIENTED_EDGE ( 'NONE', *, *, #872, .F. ) ;
#5059 = ORIENTED_EDGE ( 'NONE', *, *, #9844, .T. ) ;
#5060 = CARTESIAN_POINT ( 'NONE',  ( -13.28140389626389783, 3.000000000000000000, 13.39999999999999858 ) ) ;
#5061 = PLANE ( 'NONE',  #10226 ) ;
#5062 = EDGE_CURVE ( 'NONE', #2354, #594, #7269, .T. ) ;
#5063 = ADVANCED_FACE ( 'NONE', ( #10772 ), #6572, .F. ) ;
#5064 = DIRECTION ( 'NONE',  ( 0.000000000000000000, 1.000000000000000000, -0.000000000000000000 ) ) ;
#5065 = AXIS2_PLACEMENT_3D ( 'NONE', #8217, #10354, #1302 ) ;
#5066 = DIRECTION ( 'NONE',  ( -0.000000000000000000, -1.000000000000000000, -0.000000000000000000 ) ) ;
#5067 = DIRECTION ( 'NONE',  ( 0.000000000000000000, 1.000000000000000000, -0.000000000000000000 ) ) ;
#5068 = AXIS2_PLACEMENT_3D ( 'NONE', #9501, #4269, #4400 ) ;
#5069 = EDGE_CURVE ( 'NONE', #45, #1742, #1318, .T. ) ;
#5070 = EDGE_CURVE ( 'NONE', #525, #10812, #6639, .T. ) ;
#5071 = LINE ( 'NONE', #5966, #4933 ) ;
#5072 = DIRECTION ( 'NONE',  ( -0.000000000000000000, -1.000000000000000000, -0.000000000000000000 ) ) ;
#5073 = ORIENTED_EDGE ( 'NONE', *, *, #1932, .F. ) ;
#5074 = B_SPLINE_CURVE_WITH_KNOTS ( 'NONE', 3,
 ( #1820, #5878, #11252, #9112 ),
 .UNSPECIFIED., .F., .F.,
 ( 4, 4 ),
 ( 0.1547128134717859205, 1.000000000000000000 ),
 .UNSPECIFIED. ) ;
#5075 = CARTESIAN_POINT ( 'NONE',  ( 6.000000000000008882, 0.000000000000000000, 25.50000000000000000 ) ) ;
#5076 = CARTESIAN_POINT ( 'NONE',  ( -3.893011711613112880, 3.000000000000000000, -12.40340517008282717 ) ) ;
#5077 = CIRCLE ( 'NONE', #10792, 0.1000000000000000472 ) ;
#5078 = CIRCLE ( 'NONE', #9030, 0.1000000000000000472 ) ;
#5079 = ORIENTED_EDGE ( 'NONE', *, *, #4891, .F. ) ;
#5080 = EDGE_CURVE ( 'NONE', #1998, #2013, #3075, .T. ) ;
#5081 = LINE ( 'NONE', #9278, #10552 ) ;
#5082 = CARTESIAN_POINT ( 'NONE',  ( -2.047579527506466324, 31.33135765298363751, 9.239060114367418919 ) ) ;
#5083 = CARTESIAN_POINT ( 'NONE',  ( 1.557181465540669496, 3.000000000000000000, -14.16466328168010769 ) ) ;
#5084 = CARTESIAN_POINT ( 'NONE',  ( 10.98198414889934682, 0.000000000000000000, -9.379342464487748998 ) ) ;
#5085 = CARTESIAN_POINT ( 'NONE',  ( 20.00000000000001066, 5.249999999999972466, -5.204170427930418128E-15 ) ) ;
#5086 = ADVANCED_FACE ( 'NONE', ( #10846 ), #82, .F. ) ;
#5087 = AXIS2_PLACEMENT_3D ( 'NONE', #6170, #5142, #11552 ) ;
#5088 = AXIS2_PLACEMENT_3D ( 'NONE', #6776, #5532, #11951 ) ;
#5089 = CARTESIAN_POINT ( 'NONE',  ( 11.46847481510586775, 3.000000000000000000, 5.708888906988908829 ) ) ;
#5090 = CARTESIAN_POINT ( 'NONE',  ( 2.546103534247748712, 0.000000000000000000, -12.55526518755974585 ) ) ;
#5091 = ORIENTED_EDGE ( 'NONE', *, *, #12432, .F. ) ;
#5092 = EDGE_LOOP ( 'NONE', ( #1908, #7529, #8317, #580 ) ) ;
#5093 = DIRECTION ( 'NONE',  ( 0.000000000000000000, 0.000000000000000000, 1.000000000000000000 ) ) ;
#5094 = ORIENTED_EDGE ( 'NONE', *, *, #6118, .F. ) ;
#5095 = AXIS2_PLACEMENT_3D ( 'NONE', #2158, #4021, #926 ) ;
#5096 = ADVANCED_FACE ( 'NONE', ( #8627 ), #8412, .F. ) ;
#5097 = LINE ( 'NONE', #6070, #10070 ) ;
#5098 = DIRECTION ( 'NONE',  ( -0.000000000000000000, -1.000000000000000000, 0.000000000000000000 ) ) ;
#5099 = CARTESIAN_POINT ( 'NONE',  ( 0.000000000000000000, 9.000000000000000000, 0.000000000000000000 ) ) ;
#5100 = DIRECTION ( 'NONE',  ( 0.000000000000000000, 1.000000000000000000, 0.000000000000000000 ) ) ;
#5101 = CARTESIAN_POINT ( 'NONE',  ( -8.430890348300124515, 0.000000000000000000, 11.48836750521761019 ) ) ;
#5102 = DIRECTION ( 'NONE',  ( 0.000000000000000000, 0.000000000000000000, 1.000000000000000000 ) ) ;
#5103 = ORIENTED_EDGE ( 'NONE', *, *, #3200, .T. ) ;
#5104 = CLOSED_SHELL ( 'NONE', ( #6346, #4729, #7772, #7160, #3135, #12424, #8929, #8413, #640, #5430, #8925, #7004, #1328, #10623, #7115, #5346, #10816, #10300, #5184, #10309, #4918, #2971, #1685, #5899, #10703, #6771, #9806, #4054, #8806, #6866, #7593, #3989, #3299, #2854, #3529, #191, #12368, #8709, #5860, #11629, #2451, #2115, #2718, #10301, #7955, #4225, #1216, #3536, #4315, #8125, #8577, #4643, #4006, #9240, #369, #9532, #7870, #11032, #4551, #4151, #4639 ) ) ;
#5105 = DIRECTION ( 'NONE',  ( 0.000000000000000000, 1.000000000000000000, 0.000000000000000000 ) ) ;
#5106 = AXIS2_PLACEMENT_3D ( 'NONE', #3405, #322, #12784 ) ;
#5107 = ORIENTED_EDGE ( 'NONE', *, *, #8448, .F. ) ;
#5108 = ORIENTED_EDGE ( 'NONE', *, *, #6160, .F. ) ;
#5109 = CARTESIAN_POINT ( 'NONE',  ( 0.000000000000000000, 3.000000000000000000, 0.000000000000000000 ) ) ;
#5110 = B_SPLINE_CURVE_WITH_KNOTS ( 'NONE', 3,
 ( #6123, #4955, #825, #13497 ),
 .UNSPECIFIED., .F., .F.,
 ( 4, 4 ),
 ( 0.000000000000000000, 0.8452273900860258760 ),
 .UNSPECIFIED. ) ;
#5111 = VERTEX_POINT ( 'NONE', #3532 ) ;
#5112 = LINE ( 'NONE', #4983, #8895 ) ;
#5113 = VECTOR ( 'NONE', #11227, 1000.000000000000000 ) ;
#5114 = LINE ( 'NONE', #11180, #1432 ) ;
#5115 = VECTOR ( 'NONE', #1199, 1000.000000000000000 ) ;
#5116 = CARTESIAN_POINT ( 'NONE',  ( 8.430890348300625448, 3.000000000000000000, 11.48836750521723893 ) ) ;
#5117 = FACE_OUTER_BOUND ( 'NONE', #3391, .T. ) ;
#5118 = CARTESIAN_POINT ( 'NONE',  ( -14.16466328168009881, 3.000000000000000000, 1.557181465540760534 ) ) ;
#5119 = DIRECTION ( 'NONE',  ( 0.000000000000000000, 0.000000000000000000, -1.000000000000000000 ) ) ;
#5120 = DIRECTION ( 'NONE',  ( -0.000000000000000000, -1.000000000000000000, -0.000000000000000000 ) ) ;
#5121 = FACE_OUTER_BOUND ( 'NONE', #1179, .T. ) ;
#5122 = CARTESIAN_POINT ( 'NONE',  ( -8.100301009650792139, 9.000000000000000000, -2.575873357339267589 ) ) ;
#5123 = ORIENTED_EDGE ( 'NONE', *, *, #10875, .F. ) ;
#5124 = CARTESIAN_POINT ( 'NONE',  ( -8.369528376005813897, 9.000000000000000000, 1.483574994138650460 ) ) ;
#5125 = ORIENTED_EDGE ( 'NONE', *, *, #7422, .T. ) ;
#5126 = CIRCLE ( 'NONE', #12617, 1.500000000000000666 ) ;
#5127 = EDGE_LOOP ( 'NONE', ( #4664, #5260, #9253, #9603 ) ) ;
#5128 = CIRCLE ( 'NONE', #11284, 6.749999999999999112 ) ;
#5129 = VECTOR ( 'NONE', #9308, 1000.000000000000000 ) ;
#5130 = B_SPLINE_CURVE_WITH_KNOTS ( 'NONE', 3,
 ( #9884, #5833, #395, #5895 ),
 .UNSPECIFIED., .F., .F.,
 ( 4, 4 ),
 ( 0.000000000000000000, 0.5855695330273008592 ),
 .UNSPECIFIED. ) ;
#5131 = ADVANCED_FACE ( 'NONE', ( #9809 ), #9669, .T. ) ;
#5132 = VERTEX_POINT ( 'NONE', #5463 ) ;
#5133 = ORIENTED_EDGE ( 'NONE', *, *, #2892, .T. ) ;
#5134 = CARTESIAN_POINT ( 'NONE',  ( -5.733772933379472470, 0.000000000000000000, 13.04554897075799502 ) ) ;
#5135 = SHAPE_REPRESENTATION ( 'gear-link-2', ( #10007 ), #6949 ) ;
#5136 = CYLINDRICAL_SURFACE ( 'NONE', #3162, 12.08999999999737263 ) ;
#5137 = VECTOR ( 'NONE', #8908, 1000.000000000000000 ) ;
#5138 = DIRECTION ( 'NONE',  ( -0.000000000000000000, -1.000000000000000000, -0.000000000000000000 ) ) ;
#5139 = CIRCLE ( 'NONE', #1843, 1.600000000000000311 ) ;
#5140 = AXIS2_PLACEMENT_3D ( 'NONE', #11203, #9348, #6049 ) ;
#5141 = CARTESIAN_POINT ( 'NONE',  ( -10.67828022838850721, 3.000000000000000000, 7.077546079049267469 ) ) ;
#5142 = DIRECTION ( 'NONE',  ( -0.000000000000000000, -1.000000000000000000, -0.000000000000000000 ) ) ;
#5143 = CARTESIAN_POINT ( 'NONE',  ( 50.46378962010818015, 3.000000000000000000, -4.178819016005276943 ) ) ;
#5144 = CARTESIAN_POINT ( 'NONE',  ( -8.922136023539609440, 3.000000000000000000, 8.158651161643900807 ) ) ;
#5145 = ORIENTED_EDGE ( 'NONE', *, *, #10005, .F. ) ;
#5146 = EDGE_CURVE ( 'NONE', #1296, #9824, #440, .T. ) ;
#5147 = CARTESIAN_POINT ( 'NONE',  ( 6.749972395921142621, 0.000000000000000000, -0.01930425607464712062 ) ) ;
#5148 = EDGE_CURVE ( 'NONE', #5785, #8320, #245, .T. ) ;
#5149 = CYLINDRICAL_SURFACE ( 'NONE', #503, 3.000000000000002665 ) ;
#5150 = AXIS2_PLACEMENT_3D ( 'NONE', #12288, #2830, #6972 ) ;
#5151 = EDGE_LOOP ( 'NONE', ( #7966, #13171, #269, #6371 ) ) ;
#5152 = CARTESIAN_POINT ( 'NONE',  ( 6.553553527263006551, 9.000000000000000000, 1.616612558808879774 ) ) ;
#5153 = ADVANCED_FACE ( 'NONE', ( #2512 ), #4437, .F. ) ;
#5154 = DIRECTION ( 'NONE',  ( 0.000000000000000000, 1.000000000000000000, -0.000000000000000000 ) ) ;
#5155 = CARTESIAN_POINT ( 'NONE',  ( 33.92696780347059615, 31.33135765298343500, 14.10964106096158233 ) ) ;
#5156 = DIRECTION ( 'NONE',  ( 0.000000000000000000, 0.000000000000000000, 1.000000000000000000 ) ) ;
#5157 = LINE ( 'NONE', #7425, #2437 ) ;
#5158 = CIRCLE ( 'NONE', #11095, 1.000000000000000000 ) ;
#5159 = CARTESIAN_POINT ( 'NONE',  ( -12.98835496148321944, 3.000000000000000000, -0.5501230721522551992 ) ) ;
#5160 = VECTOR ( 'NONE', #11493, 1000.000000000000000 ) ;
#5161 = FACE_OUTER_BOUND ( 'NONE', #11995, .T. ) ;
#5162 = CARTESIAN_POINT ( 'NONE',  ( 5.051606143860418285, 0.000000000000000000, 4.477027514692275112 ) ) ;
#5163 = EDGE_CURVE ( 'NONE', #8924, #1247, #10775, .T. ) ;
#5164 = ORIENTED_EDGE ( 'NONE', *, *, #1316, .T. ) ;
#5165 = EDGE_LOOP ( 'NONE', ( #3239, #10236, #1113, #2102 ) ) ;
#5166 = ORIENTED_EDGE ( 'NONE', *, *, #1030, .F. ) ;
#5167 = CARTESIAN_POINT ( 'NONE',  ( -2.264806262022998062, 0.000000000000000000, -14.82803603298499340 ) ) ;
#5168 = ORIENTED_EDGE ( 'NONE', *, *, #7731, .F. ) ;
#5169 = AXIS2_PLACEMENT_3D ( 'NONE', #1010, #11673, #9543 ) ;
#5170 = CIRCLE ( 'NONE', #7155, 1.500000000000000444 ) ;
#5171 = EDGE_CURVE ( 'NONE', #12311, #11204, #2173, .T. ) ;
#5172 = AXIS2_PLACEMENT_3D ( 'NONE', #9445, #28, #5445 ) ;
#5173 = B_SPLINE_CURVE_WITH_KNOTS ( 'NONE', 3,
 ( #12025, #11042, #3665, #4709 ),
 .UNSPECIFIED., .F., .F.,
 ( 4, 4 ),
 ( 0.000000000000000000, 0.5855695330273008592 ),
 .UNSPECIFIED. ) ;
#5174 = CARTESIAN_POINT ( 'NONE',  ( -6.934601996837493232, 0.000000000000000000, 3.871968458191308748 ) ) ;
#5175 = CARTESIAN_POINT ( 'NONE',  ( 6.000000000000008882, 0.000000000000000000, 27.00000000000000000 ) ) ;
#5176 = CARTESIAN_POINT ( 'NONE',  ( -3.533475733155563070, 9.000000000000000000, 7.730753471893976325 ) ) ;
#5177 = CARTESIAN_POINT ( 'NONE',  ( -5.250000000000000000, 3.000000000000000000, -27.94078293894052578 ) ) ;
#5178 = LINE ( 'NONE', #10274, #8813 ) ;
#5179 = CARTESIAN_POINT ( 'NONE',  ( -13.17831234185052836, 0.000000000000000000, -4.227250083625696320 ) ) ;
#5180 = ORIENTED_EDGE ( 'NONE', *, *, #11038, .T. ) ;
#5181 = AXIS2_PLACEMENT_3D ( 'NONE', #8405, #4354, #2019 ) ;
#5182 = CARTESIAN_POINT ( 'NONE',  ( 0.000000000000000000, 3.000000000000000000, 5.000000000000000000 ) ) ;
#5183 = VECTOR ( 'NONE', #977, 1000.000000000000227 ) ;
#5184 = ADVANCED_FACE ( 'NONE', ( #1548 ), #5739, .T. ) ;
#5185 = ORIENTED_EDGE ( 'NONE', *, *, #6318, .F. ) ;
#5186 = EDGE_CURVE ( 'NONE', #9762, #3498, #2829, .T. ) ;
#5187 = VERTEX_POINT ( 'NONE', #11187 ) ;
#5188 = CARTESIAN_POINT ( 'NONE',  ( -3.893011711613112880, 3.000000000000000000, -12.40340517008282717 ) ) ;
#5189 = ORIENTED_EDGE ( 'NONE', *, *, #10821, .T. ) ;
#5190 = CARTESIAN_POINT ( 'NONE',  ( -0.8973464813148227526, 9.000000000000000000, -7.308217849399443189 ) ) ;
#5191 =( GEOMETRIC_REPRESENTATION_CONTEXT ( 3 ) GLOBAL_UNCERTAINTY_ASSIGNED_CONTEXT ( ( #10117 ) ) GLOBAL_UNIT_ASSIGNED_CONTEXT ( ( #12492, #2543, #5492 ) ) REPRESENTATION_CONTEXT ( 'NONE', 'WORKASPACE' ) );
#5192 = CYLINDRICAL_SURFACE ( 'NONE', #3622, 8.500000000000000000 ) ;
#5193 = CARTESIAN_POINT ( 'NONE',  ( 2.623034112301249721, 0.000000000000000000, -7.496701717520498853 ) ) ;
#5194 = DIRECTION ( 'NONE',  ( 0.000000000000000000, 0.000000000000000000, 1.000000000000000000 ) ) ;
#5195 = DIRECTION ( 'NONE',  ( 0.000000000000000000, 0.000000000000000000, 1.000000000000000000 ) ) ;
#5196 = DIRECTION ( 'NONE',  ( 0.000000000000000000, 0.000000000000000000, -1.000000000000000000 ) ) ;
#5197 = CARTESIAN_POINT ( 'NONE',  ( -7.723663868796776910, 3.000000000000000000, -11.13895890373326303 ) ) ;
#5198 = LINE ( 'NONE', #9328, #6050 ) ;
#5199 = ORIENTED_EDGE ( 'NONE', *, *, #1970, .T. ) ;
#5200 = CARTESIAN_POINT ( 'NONE',  ( 8.922136023539611216, 3.000000000000000000, -8.158651161643899030 ) ) ;
#5201 = ORIENTED_EDGE ( 'NONE', *, *, #12054, .T. ) ;
#5202 = EDGE_CURVE ( 'NONE', #12679, #2677, #376, .T. ) ;
#5203 = DIRECTION ( 'NONE',  ( -0.000000000000000000, -1.000000000000000000, -0.000000000000000000 ) ) ;
#5204 = ORIENTED_EDGE ( 'NONE', *, *, #7702, .T. ) ;
#5205 = EDGE_LOOP ( 'NONE', ( #5861, #13540, #1293, #12519 ) ) ;
#5206 = ORIENTED_EDGE ( 'NONE', *, *, #11889, .F. ) ;
#5207 = DIRECTION ( 'NONE',  ( -0.000000000000000000, -1.000000000000000000, -0.000000000000000000 ) ) ;
#5208 = CARTESIAN_POINT ( 'NONE',  ( 6.329356821613516537, 0.000000000000000000, -12.30759122141987305 ) ) ;
#5209 = CARTESIAN_POINT ( 'NONE',  ( 2.719999999999997087, 2.000000000000000000, -6.000000000000000000 ) ) ;
#5210 = CYLINDRICAL_SURFACE ( 'NONE', #13229, 2.999999999999999112 ) ;
#5211 = CARTESIAN_POINT ( 'NONE',  ( 8.430890348300565051, 3.000000000000000000, -11.48836750521728334 ) ) ;
#5212 = ORIENTED_EDGE ( 'NONE', *, *, #7755, .T. ) ;
#5213 = DIRECTION ( 'NONE',  ( -0.000000000000000000, -1.000000000000000000, -0.000000000000000000 ) ) ;
#5214 = CARTESIAN_POINT ( 'NONE',  ( 53.78299299645824050, 0.000000000000000000, -4.528231303176834643 ) ) ;
#5215 = ORIENTED_EDGE ( 'NONE', *, *, #11732, .T. ) ;
#5216 = DIRECTION ( 'NONE',  ( -0.000000000000000000, -1.000000000000000000, -0.000000000000000000 ) ) ;
#5217 = DIRECTION ( 'NONE',  ( 1.000000000000000000, -0.000000000000000000, 0.000000000000000000 ) ) ;
#5218 = CARTESIAN_POINT ( 'NONE',  ( 5.250000000000000000, 3.000000000000000000, -29.44078293894052933 ) ) ;
#5219 = DIRECTION ( 'NONE',  ( 0.000000000000000000, 1.000000000000000000, -0.000000000000000000 ) ) ;
#5220 = EDGE_CURVE ( 'NONE', #11515, #1266, #4989, .T. ) ;
#5221 = CARTESIAN_POINT ( 'NONE',  ( -8.883544964652065445, 3.000000000000000000, -12.08646469655229438 ) ) ;
#5222 = EDGE_CURVE ( 'NONE', #1728, #6683, #7057, .T. ) ;
#5223 = CARTESIAN_POINT ( 'NONE',  ( 23.99887587215152251, 3.000000000000000000, 5.000000000000000888 ) ) ;
#5224 = CARTESIAN_POINT ( 'NONE',  ( 12.90250726680438476, 0.000000000000000000, 4.728042766759046778 ) ) ;
#5225 = VERTEX_POINT ( 'NONE', #2922 ) ;
#5226 = ORIENTED_EDGE ( 'NONE', *, *, #1993, .T. ) ;
#5227 = LINE ( 'NONE', #10327, #11498 ) ;
#5228 = ORIENTED_EDGE ( 'NONE', *, *, #5265, .F. ) ;
#5229 = CARTESIAN_POINT ( 'NONE',  ( 4.355042381134426321, 9.000000000000000000, 7.299562031966228659 ) ) ;
#5230 =( LENGTH_UNIT ( ) NAMED_UNIT ( * ) SI_UNIT ( .MILLI., .METRE. ) );
#5231 = DIRECTION ( 'NONE',  ( 0.000000000000000000, 0.000000000000000000, 1.000000000000000000 ) ) ;
#5232 = EDGE_CURVE ( 'NONE', #9256, #1608, #12866, .T. ) ;
#5233 = DIRECTION ( 'NONE',  ( 0.000000000000000000, 0.000000000000000000, 1.000000000000000000 ) ) ;
#5234 = FACE_OUTER_BOUND ( 'NONE', #3158, .T. ) ;
#5235 = PRODUCT_DEFINITION_SHAPE ( 'NONE', 'NONE',  #13615 ) ;
#5236 = ADVANCED_FACE ( 'NONE', ( #1902 ), #6329, .F. ) ;
#5237 = CARTESIAN_POINT ( 'NONE',  ( 0.8653219153705552502, 9.000000000000000000, -7.312626806738413698 ) ) ;
#5238 = CARTESIAN_POINT ( 'NONE',  ( 10.00000000000001954, 8.000000000000007105, -10.00000000000000000 ) ) ;
#5239 = VERTEX_POINT ( 'NONE', #8146 ) ;
#5240 = EDGE_CURVE ( 'NONE', #7348, #1088, #6095, .T. ) ;
#5241 = DIRECTION ( 'NONE',  ( 0.000000000000000000, 0.000000000000000000, 1.000000000000000000 ) ) ;
#5242 = EDGE_CURVE ( 'NONE', #2397, #4803, #2428, .T. ) ;
#5243 = VERTEX_POINT ( 'NONE', #8087 ) ;
#5244 = B_SPLINE_CURVE_WITH_KNOTS ( 'NONE', 3,
 ( #1243, #3432, #6476, #11847 ),
 .UNSPECIFIED., .F., .F.,
 ( 4, 4 ),
 ( 0.000000000000000000, 0.8724294488011775650 ),
 .UNSPECIFIED. ) ;
#5245 = VERTEX_POINT ( 'NONE', #9182 ) ;
#5246 = DIRECTION ( 'NONE',  ( -0.000000000000000000, -1.000000000000000000, -0.000000000000000000 ) ) ;
#5247 = VERTEX_POINT ( 'NONE', #5948 ) ;
#5248 = DIRECTION ( 'NONE',  ( -0.000000000000000000, -1.000000000000000000, -0.000000000000000000 ) ) ;
#5249 = LINE ( 'NONE', #4146, #5613 ) ;
#5250 = DIRECTION ( 'NONE',  ( 0.000000000000000000, 0.000000000000000000, 1.000000000000000000 ) ) ;
#5251 = DIRECTION ( 'NONE',  ( 0.000000000000000000, 0.000000000000000000, -1.000000000000000000 ) ) ;
#5252 = DIRECTION ( 'NONE',  ( 0.6923076923076925127, 0.000000000000000000, 0.7216024245882197707 ) ) ;
#5253 = CARTESIAN_POINT ( 'NONE',  ( -5.976238463952679325, 9.000000000000000000, -3.138004751744733589 ) ) ;
#5254 = DIRECTION ( 'NONE',  ( -0.000000000000000000, -1.000000000000000000, -0.000000000000000000 ) ) ;
#5255 = CARTESIAN_POINT ( 'NONE',  ( -7.077546079049271910, 0.000000000000000000, -10.67828022838850544 ) ) ;
#5256 = VERTEX_POINT ( 'NONE', #6026 ) ;
#5257 = DIRECTION ( 'NONE',  ( 0.000000000000000000, 1.000000000000000000, -0.000000000000000000 ) ) ;
#5258 = EDGE_LOOP ( 'NONE', ( #1748, #13382, #1795, #5989 ) ) ;
#5259 = VERTEX_POINT ( 'NONE', #10292 ) ;
#5260 = ORIENTED_EDGE ( 'NONE', *, *, #7985, .F. ) ;
#5261 = EDGE_LOOP ( 'NONE', ( #5674, #4612, #10599, #3412 ) ) ;
#5262 = DIRECTION ( 'NONE',  ( 0.000000000000000000, 0.000000000000000000, 1.000000000000000000 ) ) ;
#5263 = PRESENTATION_STYLE_ASSIGNMENT (( #9407 ) ) ;
#5264 = EDGE_CURVE ( 'NONE', #8754, #9963, #8570, .T. ) ;
#5265 = EDGE_CURVE ( 'NONE', #7779, #1278, #3085, .T. ) ;
#5266 = CARTESIAN_POINT ( 'NONE',  ( 5.170206418547604876, 0.000000000000000000, -13.27898586450069196 ) ) ;
#5267 = DIRECTION ( 'NONE',  ( -0.000000000000000000, -1.000000000000000000, -0.000000000000000000 ) ) ;
#5268 = CARTESIAN_POINT ( 'NONE',  ( -6.970598036433426792, 0.000000000000000000, -10.97318381393771780 ) ) ;
#5269 = DIRECTION ( 'NONE',  ( -0.000000000000000000, -1.000000000000000000, -0.000000000000000000 ) ) ;
#5270 = AXIS2_PLACEMENT_3D ( 'NONE', #11640, #10536, #11704 ) ;
#5271 = ORIENTED_EDGE ( 'NONE', *, *, #490, .F. ) ;
#5272 = VERTEX_POINT ( 'NONE', #11047 ) ;
#5273 = CARTESIAN_POINT ( 'NONE',  ( -12.98835496148299207, 0.000000000000000000, 0.5501230721524459355 ) ) ;
#5274 = B_SPLINE_CURVE_WITH_KNOTS ( 'NONE', 3,
 ( #12973, #5804, #5601, #10006 ),
 .UNSPECIFIED., .F., .F.,
 ( 4, 4 ),
 ( 0.000000000000000000, 0.8724294488011774540 ),
 .UNSPECIFIED. ) ;
#5275 = ORIENTED_EDGE ( 'NONE', *, *, #12451, .T. ) ;
#5276 = LINE ( 'NONE', #2052, #9544 ) ;
#5277 = VECTOR ( 'NONE', #1957, 1000.000000000000000 ) ;
#5278 = CIRCLE ( 'NONE', #10992, 14.25000000000000178 ) ;
#5279 = FACE_OUTER_BOUND ( 'NONE', #3556, .T. ) ;
#5280 = SHAPE_DEFINITION_REPRESENTATION ( #3140, #11353 ) ;
#5281 = PLANE ( 'NONE',  #2882 ) ;
#5282 = DIRECTION ( 'NONE',  ( 0.000000000000000000, 0.000000000000000000, 1.000000000000000000 ) ) ;
#5283 = CARTESIAN_POINT ( 'NONE',  ( 0.000000000000000000, 0.000000000000000000, 0.000000000000000000 ) ) ;
#5284 = CARTESIAN_POINT ( 'NONE',  ( -11.35348746973813761, 0.000000000000000000, -6.343077501554963860 ) ) ;
#5285 = DIRECTION ( 'NONE',  ( 0.000000000000000000, 1.000000000000000000, 0.000000000000000000 ) ) ;
#5286 = VECTOR ( 'NONE', #602, 1000.000000000000000 ) ;
#5287 = ORIENTED_EDGE ( 'NONE', *, *, #6955, .T. ) ;
#5288=STYLED_ITEM('',(#13663),#4005);
#5289 = ORIENTED_EDGE ( 'NONE', *, *, #8235, .F. ) ;
#5290 = EDGE_LOOP ( 'NONE', ( #13092, #3889, #9582, #12281 ) ) ;
#5291 = DIRECTION ( 'NONE',  ( 0.000000000000000000, 1.000000000000000000, 0.000000000000000000 ) ) ;
#5292 = ADVANCED_FACE ( 'NONE', ( #4845 ), #12304, .F. ) ;
#5293 = ORIENTED_EDGE ( 'NONE', *, *, #3629, .F. ) ;
#5294 = FACE_BOUND ( 'NONE', #8165, .T. ) ;
#5295 = AXIS2_PLACEMENT_3D ( 'NONE', #6301, #7412, #10513 ) ;
#5296 = CARTESIAN_POINT ( 'NONE',  ( 6.217402469309262436, 0.000000000000000000, -13.03533457366732939 ) ) ;
#5297 = CARTESIAN_POINT ( 'NONE',  ( 5.784789447945496654, 0.000000000000000000, -12.25836857253663581 ) ) ;
#5298 = CIRCLE ( 'NONE', #3971, 0.9999999999999991118 ) ;
#5299 = LINE ( 'NONE', #10804, #3828 ) ;
#5300 = DIRECTION ( 'NONE',  ( -0.000000000000000000, -1.000000000000000000, -0.000000000000000000 ) ) ;
#5301 = CYLINDRICAL_SURFACE ( 'NONE', #1664, 2.999999999999999112 ) ;
#5302 = ORIENTED_EDGE ( 'NONE', *, *, #6725, .F. ) ;
#5303 = ORIENTED_EDGE ( 'NONE', *, *, #6449, .T. ) ;
#5304 = ORIENTED_EDGE ( 'NONE', *, *, #8912, .T. ) ;
#5305 = ORIENTED_EDGE ( 'NONE', *, *, #2516, .T. ) ;
#5306 = CARTESIAN_POINT ( 'NONE',  ( -8.771102293099080072, 0.000000000000000000, -10.33484986938307770 ) ) ;
#5307 = VECTOR ( 'NONE', #8546, 1000.000000000000000 ) ;
#5308 = EDGE_CURVE ( 'NONE', #7949, #6730, #5883, .T. ) ;
#5309 = EDGE_CURVE ( 'NONE', #6406, #4317, #3508, .T. ) ;
#5310 = VERTEX_POINT ( 'NONE', #11258 ) ;
#5311 = CYLINDRICAL_SURFACE ( 'NONE', #12873, 12.08999999999737440 ) ;
#5312 = EDGE_CURVE ( 'NONE', #7170, #2755, #7281, .T. ) ;
#5313 = EDGE_CURVE ( 'NONE', #8988, #7608, #12114, .T. ) ;
#5314 = CARTESIAN_POINT ( 'NONE',  ( 5.250000000000000000, 3.000000000000000000, -26.44078293894052578 ) ) ;
#5315 = CARTESIAN_POINT ( 'NONE',  ( -5.250000000000000000, 3.000000000000000000, -26.44078293894052578 ) ) ;
#5316 = DIRECTION ( 'NONE',  ( 0.000000000000000000, -0.000000000000000000, 1.000000000000000000 ) ) ;
#5317 = CARTESIAN_POINT ( 'NONE',  ( 51.83140210808490167, 0.000000000000000000, -12.77460472465662988 ) ) ;
#5318 = VECTOR ( 'NONE', #1141, 1000.000000000000000 ) ;
#5319 = DIRECTION ( 'NONE',  ( 0.000000000000000000, 0.000000000000000000, -1.000000000000000000 ) ) ;
#5320 = DIRECTION ( 'NONE',  ( 0.000000000000000000, 0.000000000000000000, 1.000000000000000000 ) ) ;
#5321 = ORIENTED_EDGE ( 'NONE', *, *, #13340, .F. ) ;
#5322 = CARTESIAN_POINT ( 'NONE',  ( 13.04554897075796838, 3.000000000000000000, -5.733772933379540859 ) ) ;
#5323 = B_SPLINE_SURFACE_WITH_KNOTS ( 'NONE', 3, 1, ( 
 ( #10467, #2959 ),
 ( #827, #11367 ),
 ( #11426, #1929 ),
 ( #6124, #12604 ) ),
 .UNSPECIFIED., .F., .F., .F.,
 ( 4, 4 ),
 ( 2, 2 ),
 ( 0.1818127957067485756, 0.2112308727645026418 ),
 ( 0.000000000000000000, 1.000000000000000000 ),
 .UNSPECIFIED. ) ;
#5324 = ORIENTED_EDGE ( 'NONE', *, *, #12397, .T. ) ;
#5325 = ORIENTED_EDGE ( 'NONE', *, *, #4748, .F. ) ;
#5326 = ADVANCED_FACE ( 'NONE', ( #6543 ), #10932, .F. ) ;
#5327 = TOROIDAL_SURFACE ( 'NONE', #5764, 3.400000000000001243, 0.1000000000000000056 ) ;
#5328 = EDGE_LOOP ( 'NONE', ( #7337, #13110, #11975, #12262 ) ) ;
#5329 = AXIS2_PLACEMENT_3D ( 'NONE', #10813, #1384, #5580 ) ;
#5330 = CIRCLE ( 'NONE', #12821, 14.25000000000000178 ) ;
#5331 = AXIS2_PLACEMENT_3D ( 'NONE', #4752, #6878, #11086 ) ;
#5332 = CARTESIAN_POINT ( 'NONE',  ( -5.065227977808753224, 9.000000000000000000, -4.461610195077944319 ) ) ;
#5333 = EDGE_CURVE ( 'NONE', #5245, #3720, #11880, .T. ) ;
#5334 = B_SPLINE_CURVE_WITH_KNOTS ( 'NONE', 3,
 ( #11181, #13046, #1544, #8081 ),
 .UNSPECIFIED., .F., .F.,
 ( 4, 4 ),
 ( 0.000000000000000000, 0.8724294488011774540 ),
 .UNSPECIFIED. ) ;
#5335 = LINE ( 'NONE', #3007, #953 ) ;
#5336 = DIRECTION ( 'NONE',  ( -0.000000000000000000, -1.000000000000000000, -0.000000000000000000 ) ) ;
#5337 = FACE_OUTER_BOUND ( 'NONE', #6103, .T. ) ;
#5338 = VECTOR ( 'NONE', #611, 1000.000000000000000 ) ;
#5339 = CARTESIAN_POINT ( 'NONE',  ( 41.67875868938293138, 3.000000000000000000, -6.066649533482935119 ) ) ;
#5340 = CIRCLE ( 'NONE', #7983, 3.100000000000000977 ) ;
#5341 = AXIS2_PLACEMENT_3D ( 'NONE', #6156, #5257, #2925 ) ;
#5342 = VERTEX_POINT ( 'NONE', #13536 ) ;
#5343 = ORIENTED_EDGE ( 'NONE', *, *, #7094, .T. ) ;
#5344 = ADVANCED_FACE ( 'NONE', ( #925 ), #7506, .F. ) ;
#5345 = DIRECTION ( 'NONE',  ( -0.000000000000000000, -1.000000000000000000, -0.000000000000000000 ) ) ;
#5346 = ADVANCED_FACE ( 'NONE', ( #3364 ), #3443, .T. ) ;
#5347 = ORIENTED_EDGE ( 'NONE', *, *, #11545, .T. ) ;
#5348 = FACE_OUTER_BOUND ( 'NONE', #5761, .T. ) ;
#5349 = VECTOR ( 'NONE', #13192, 1000.000000000000000 ) ;
#5350=STYLED_ITEM('',(#13628),#8567);
#5351 = CARTESIAN_POINT ( 'NONE',  ( -8.222660081691577361, 0.000000000000000000, -8.549999999999998934 ) ) ;
#5352 = DIRECTION ( 'NONE',  ( 0.000000000000000000, 0.000000000000000000, 1.000000000000000000 ) ) ;
#5353 = CARTESIAN_POINT ( 'NONE',  ( 12.90250726680438476, 0.000000000000000000, 4.728042766759046778 ) ) ;
#5354 = DIRECTION ( 'NONE',  ( 0.000000000000000000, 1.000000000000000000, 0.000000000000000000 ) ) ;
#5355 = DIRECTION ( 'NONE',  ( 0.000000000000000000, 0.000000000000000000, -1.000000000000000000 ) ) ;
#5356 = AXIS2_PLACEMENT_3D ( 'NONE', #3890, #9337, #4103 ) ;
#5357 =( LENGTH_UNIT ( ) NAMED_UNIT ( * ) SI_UNIT ( .MILLI., .METRE. ) );
#5358 = AXIS2_PLACEMENT_3D ( 'NONE', #12945, #1172, #1301 ) ;
#5359 = VERTEX_POINT ( 'NONE', #10743 ) ;
#5360 = EDGE_LOOP ( 'NONE', ( #8753, #5663, #8991, #10419 ) ) ;
#5361 = EDGE_LOOP ( 'NONE', ( #3409, #7730, #10004, #2463, #10754, #828, #6245, #8944, #13154, #7903, #308, #705, #13434, #2190, #10115, #13126 ) ) ;
#5362 = CARTESIAN_POINT ( 'NONE',  ( -1.958311002203252160, 0.000000000000000000, -14.87484884897975768 ) ) ;
#5363 = ORIENTED_EDGE ( 'NONE', *, *, #860, .F. ) ;
#5364 = FACE_OUTER_BOUND ( 'NONE', #10675, .T. ) ;
#5365 = CIRCLE ( 'NONE', #8438, 1.499999999686092877 ) ;
#5366 = VECTOR ( 'NONE', #11895, 1000.000000000000000 ) ;
#5367 = CARTESIAN_POINT ( 'NONE',  ( 5.170206418547604876, 3.000000000000000000, -13.27898586450069196 ) ) ;
#5368 = AXIS2_PLACEMENT_3D ( 'NONE', #8965, #1410, #6908 ) ;
#5369 = DIRECTION ( 'NONE',  ( 0.000000000000000000, 0.000000000000000000, -1.000000000000000000 ) ) ;
#5370 = CARTESIAN_POINT ( 'NONE',  ( -8.100301009650799244, 9.000000000000000000, -2.575873357339268033 ) ) ;
#5371 = CARTESIAN_POINT ( 'NONE',  ( -5.170206418547117266, 3.000000000000000000, 13.27898586450088203 ) ) ;
#5372 = CARTESIAN_POINT ( 'NONE',  ( -9.573149624528719315, 3.000000000000000000, -8.795158114916407754 ) ) ;
#5373 = EDGE_CURVE ( 'NONE', #846, #1437, #4020, .T. ) ;
#5374 = VERTEX_POINT ( 'NONE', #12452 ) ;
#5375 = LINE ( 'NONE', #6611, #9954 ) ;
#5376 = ORIENTED_EDGE ( 'NONE', *, *, #9364, .T. ) ;
#5377 = ORIENTED_EDGE ( 'NONE', *, *, #2557, .T. ) ;
#5378=STYLED_ITEM('',(#13635),#13227);
#5379 = ORIENTED_EDGE ( 'NONE', *, *, #2613, .T. ) ;
#5380 = CIRCLE ( 'NONE', #9999, 3.000000000000000000 ) ;
#5381 = FACE_OUTER_BOUND ( 'NONE', #5393, .T. ) ;
#5382 = ORIENTED_EDGE ( 'NONE', *, *, #12741, .T. ) ;
#5383 = CARTESIAN_POINT ( 'NONE',  ( -8.352599575481674421, 3.000000000000000000, 31.00000000000000000 ) ) ;
#5384 = DIRECTION ( 'NONE',  ( -0.000000000000000000, -1.000000000000000000, -0.000000000000000000 ) ) ;
#5385 = DIRECTION ( 'NONE',  ( 0.000000000000000000, 0.000000000000000000, -1.000000000000000000 ) ) ;
#5386 = CARTESIAN_POINT ( 'NONE',  ( 6.970598036433451661, 3.000000000000000000, -10.97318381393796294 ) ) ;
#5387 = FACE_OUTER_BOUND ( 'NONE', #13243, .T. ) ;
#5388 = AXIS2_PLACEMENT_3D ( 'NONE', #3701, #2813, #7901 ) ;
#5389 = ADVANCED_FACE ( 'NONE', ( #5434 ), #9934, .F. ) ;
#5390 = CARTESIAN_POINT ( 'NONE',  ( -5.975392301194330180, 9.000000000000000000, -6.045220165289885372 ) ) ;
#5391 = DIRECTION ( 'NONE',  ( 1.370446048119726253E-16, -0.000000000000000000, 1.000000000000000000 ) ) ;
#5392 = ADVANCED_FACE ( 'NONE', ( #7202 ), #11643, .T. ) ;
#5393 = EDGE_LOOP ( 'NONE', ( #10656, #3593, #3160, #7988 ) ) ;
#5394 = B_SPLINE_CURVE_WITH_KNOTS ( 'NONE', 2,
 ( #2359, #8481, #5448 ),
 .UNSPECIFIED., .F., .F.,
 ( 3, 3 ),
 ( 0.000000000000000000, 1.000000000000000000 ),
 .UNSPECIFIED. ) ;
#5395 = CARTESIAN_POINT ( 'NONE',  ( 3.555260608155774271, 9.000000000000000000, 7.720759160088842776 ) ) ;
#5396 = EDGE_LOOP ( 'NONE', ( #1996, #359, #9297, #1867 ) ) ;
#5397 = VERTEX_POINT ( 'NONE', #11708 ) ;
#5398 = EDGE_CURVE ( 'NONE', #4831, #3424, #6376, .T. ) ;
#5399 = ORIENTED_EDGE ( 'NONE', *, *, #11804, .T. ) ;
#5400 = CARTESIAN_POINT ( 'NONE',  ( 2.999999999999997335, 0.000000000000000000, -7.000000000000001776 ) ) ;
#5401 =( NAMED_UNIT ( * ) PLANE_ANGLE_UNIT ( ) SI_UNIT ( $, .RADIAN. ) );
#5402 = CARTESIAN_POINT ( 'NONE',  ( -6.749999880766614169, 9.000000000000000000, -0.001268720102703522860 ) ) ;
#5403 = ADVANCED_FACE ( 'NONE', ( #6913 ), #5668, .F. ) ;
#5404 = CARTESIAN_POINT ( 'NONE',  ( 8.914835885878215294, 3.000000000000000000, 11.11702303352197418 ) ) ;
#5405 = CARTESIAN_POINT ( 'NONE',  ( -10.67828022838850721, 0.000000000000000000, 7.077546079049267469 ) ) ;
#5406 = AXIS2_PLACEMENT_3D ( 'NONE', #6874, #9149, #5845 ) ;
#5407 = DIRECTION ( 'NONE',  ( 0.000000000000000000, 0.000000000000000000, -1.000000000000000000 ) ) ;
#5408 = ORIENTED_EDGE ( 'NONE', *, *, #6581, .T. ) ;
#5409 = EDGE_CURVE ( 'NONE', #11196, #3086, #9037, .T. ) ;
#5410 = ORIENTED_EDGE ( 'NONE', *, *, #3659, .T. ) ;
#5411 = EDGE_CURVE ( 'NONE', #7143, #5856, #12160, .T. ) ;
#5412 = CARTESIAN_POINT ( 'NONE',  ( 45.60964950616533287, 3.000000000000000000, -14.50984893380129392 ) ) ;
#5413 = B_SPLINE_CURVE_WITH_KNOTS ( 'NONE', 3,
 ( #7723, #4495, #12906, #3450 ),
 .UNSPECIFIED., .F., .F.,
 ( 4, 4 ),
 ( 0.000000000000000000, 0.8452273900860258760 ),
 .UNSPECIFIED. ) ;
#5414 = ORIENTED_EDGE ( 'NONE', *, *, #1788, .F. ) ;
#5415 = CARTESIAN_POINT ( 'NONE',  ( -14.90895795148411374, 0.000000000000000000, -1.650143266773683726 ) ) ;
#5416 = CARTESIAN_POINT ( 'NONE',  ( 0.000000000000000000, 2.900000000000000355, 0.000000000000000000 ) ) ;
#5417 = CARTESIAN_POINT ( 'NONE',  ( 0.000000000000000000, 3.000000000000000000, 0.000000000000000000 ) ) ;
#5418 = CARTESIAN_POINT ( 'NONE',  ( 5.571313494980132397, 3.000000000000000000, -10.72979803820131472 ) ) ;
#5419 = B_SPLINE_CURVE_WITH_KNOTS ( 'NONE', 3,
 ( #3077, #3215, #6180, #10460 ),
 .UNSPECIFIED., .F., .F.,
 ( 4, 4 ),
 ( 0.1547128134717859205, 1.000000000000000000 ),
 .UNSPECIFIED. ) ;
#5420 = DIRECTION ( 'NONE',  ( -0.000000000000000000, -1.000000000000000000, -0.000000000000000000 ) ) ;
#5421 = DIRECTION ( 'NONE',  ( 0.000000000000000000, 0.000000000000000000, 1.000000000000000000 ) ) ;
#5422 = FACE_OUTER_BOUND ( 'NONE', #4481, .T. ) ;
#5423 = EDGE_LOOP ( 'NONE', ( #566, #11759, #5968, #10470 ) ) ;
#5424 = ORIENTED_EDGE ( 'NONE', *, *, #2150, .F. ) ;
#5425 = ORIENTED_EDGE ( 'NONE', *, *, #12432, .T. ) ;
#5426 = FACE_OUTER_BOUND ( 'NONE', #9048, .T. ) ;
#5427 = VERTEX_POINT ( 'NONE', #4782 ) ;
#5428 = DIRECTION ( 'NONE',  ( 0.000000000000000000, 0.000000000000000000, -1.000000000000000000 ) ) ;
#5429 = PRODUCT_DEFINITION_SHAPE ( 'NONE', 'NONE',  #4289 ) ;
#5430 = ADVANCED_FACE ( 'NONE', ( #13117 ), #6412, .T. ) ;
#5431 = DIRECTION ( 'NONE',  ( 0.000000000000000000, 1.000000000000000000, 0.000000000000000000 ) ) ;
#5432 = ADVANCED_FACE ( 'NONE', ( #7866 ), #4330, .F. ) ;
#5433 = CARTESIAN_POINT ( 'NONE',  ( 13.50000000000000355, 0.000000000000000000, -7.050000000000000711 ) ) ;
#5434 = FACE_OUTER_BOUND ( 'NONE', #8056, .T. ) ;
#5435 = FACE_OUTER_BOUND ( 'NONE', #7622, .T. ) ;
#5436 = DIRECTION ( 'NONE',  ( -0.000000000000000000, -1.000000000000000000, -0.000000000000000000 ) ) ;
#5437 = VERTEX_POINT ( 'NONE', #10079 ) ;
#5438 = DIRECTION ( 'NONE',  ( -0.000000000000000000, -1.000000000000000000, -0.000000000000000000 ) ) ;
#5439 = ORIENTED_EDGE ( 'NONE', *, *, #535, .F. ) ;
#5440 = VERTEX_POINT ( 'NONE', #9116 ) ;
#5441 = VERTEX_POINT ( 'NONE', #11949 ) ;
#5442 = DIRECTION ( 'NONE',  ( 0.000000000000000000, 0.000000000000000000, -1.000000000000000000 ) ) ;
#5443 = ORIENTED_EDGE ( 'NONE', *, *, #12857, .F. ) ;
#5444 = AXIS2_PLACEMENT_3D ( 'NONE', #6621, #8743, #12958 ) ;
#5445 = DIRECTION ( 'NONE',  ( 0.000000000000000000, 0.000000000000000000, 1.000000000000000000 ) ) ;
#5446 = FACE_OUTER_BOUND ( 'NONE', #5971, .T. ) ;
#5447 = CARTESIAN_POINT ( 'NONE',  ( -7.798201703419555209, 0.000000000000000000, -30.99999999999999289 ) ) ;
#5448 = CARTESIAN_POINT ( 'NONE',  ( -9.375397774054503586, 3.000000000000000000, -11.70905276178452503 ) ) ;
#5449 = DIRECTION ( 'NONE',  ( 0.000000000000000000, 1.000000000000000000, 0.000000000000000000 ) ) ;
#5450 = DIRECTION ( 'NONE',  ( -0.000000000000000000, -1.000000000000000000, -0.000000000000000000 ) ) ;
#5451 = FACE_OUTER_BOUND ( 'NONE', #8722, .T. ) ;
#5452 = DIRECTION ( 'NONE',  ( 1.000000000000000000, 0.000000000000000000, 0.000000000000000000 ) ) ;
#5453 = ORIENTED_EDGE ( 'NONE', *, *, #4130, .F. ) ;
#5454 = DIRECTION ( 'NONE',  ( 0.000000000000000000, 0.000000000000000000, 1.000000000000000000 ) ) ;
#5455 = ORIENTED_EDGE ( 'NONE', *, *, #210, .T. ) ;
#5456 = ORIENTED_EDGE ( 'NONE', *, *, #11051, .F. ) ;
#5457 = EDGE_LOOP ( 'NONE', ( #13400, #11668, #7878, #3658 ) ) ;
#5458 = EDGE_CURVE ( 'NONE', #9693, #9925, #11669, .T. ) ;
#5459 = LINE ( 'NONE', #120, #13511 ) ;
#5460 = PRODUCT_DEFINITION ( 'UNKNOWN', '', #12680, #7098 ) ;
#5461 = CARTESIAN_POINT ( 'NONE',  ( 6.017756925049591921, 0.000000000000000000, -11.52330688609011844 ) ) ;
#5462 = LINE ( 'NONE', #10912, #12418 ) ;
#5463 = CARTESIAN_POINT ( 'NONE',  ( 31.00000000000000000, 3.000000000000000000, -4.000000001073670930 ) ) ;
#5464 = DIRECTION ( 'NONE',  ( 0.000000000000000000, 0.000000000000000000, 1.000000000000000000 ) ) ;
#5466 = CARTESIAN_POINT ( 'NONE',  ( 0.9098489087730803337, 0.000000000000000000, 7.307220250892556557 ) ) ;
#5465 = B_SPLINE_CURVE_WITH_KNOTS ( 'NONE', 2,
 ( #10080, #7056, #513 ),
 .UNSPECIFIED., .F., .F.,
 ( 3, 3 ),
 ( 0.000000000000000000, 1.000000000000000000 ),
 .UNSPECIFIED. ) ;
#5467 = ORIENTED_EDGE ( 'NONE', *, *, #1733, .F. ) ;
#5468 = EDGE_LOOP ( 'NONE', ( #10276, #3039, #8065, #4243 ) ) ;
#5469 = CARTESIAN_POINT ( 'NONE',  ( 4.201465772524378472, 0.000000000000000000, 6.047394330962382547 ) ) ;
#5470 = ADVANCED_FACE ( 'NONE', ( #10012 ), #6710, .T. ) ;
#5471 = EDGE_CURVE ( 'NONE', #4097, #4297, #8969, .T. ) ;
#5472 = ORIENTED_EDGE ( 'NONE', *, *, #987, .F. ) ;
#5473 = DIRECTION ( 'NONE',  ( 0.000000000000000000, 1.000000000000000000, -0.000000000000000000 ) ) ;
#5474 = CARTESIAN_POINT ( 'NONE',  ( 0.000000000000000000, 1.000000000000000000, -2.500000000000000444 ) ) ;
#5475 = EDGE_CURVE ( 'NONE', #13401, #7860, #3812, .T. ) ;
#5476 = EDGE_CURVE ( 'NONE', #10281, #8802, #10344, .T. ) ;
#5477 = DIRECTION ( 'NONE',  ( 0.000000000000000000, 0.000000000000000000, -1.000000000000000000 ) ) ;
#5478 = LINE ( 'NONE', #5623, #13215 ) ;
#5479 = AXIS2_PLACEMENT_3D ( 'NONE', #7423, #2180, #11421 ) ;
#5480 = CARTESIAN_POINT ( 'NONE',  ( 0.000000000000000000, 0.000000000000000000, 0.000000000000000000 ) ) ;
#5481 = PRESENTATION_STYLE_ASSIGNMENT (( #1290 ) ) ;
#5482 = ORIENTED_EDGE ( 'NONE', *, *, #5062, .T. ) ;
#5483 = ORIENTED_EDGE ( 'NONE', *, *, #2145, .F. ) ;
#5484 = ORIENTED_EDGE ( 'NONE', *, *, #1716, .T. ) ;
#5485 = ORIENTED_EDGE ( 'NONE', *, *, #10374, .F. ) ;
#5486 = CARTESIAN_POINT ( 'NONE',  ( 30.73000000000000043, 3.000000000000000000, -2.499999999999995115 ) ) ;
#5487 = AXIS2_PLACEMENT_3D ( 'NONE', #13275, #8032, #7073 ) ;
#5488 = EDGE_CURVE ( 'NONE', #1714, #1838, #6841, .T. ) ;
#5489 = VECTOR ( 'NONE', #11182, 1000.000000000000000 ) ;
#5490 = VERTEX_POINT ( 'NONE', #5735 ) ;
#5491 = FACE_OUTER_BOUND ( 'NONE', #6035, .T. ) ;
#5492 =( NAMED_UNIT ( * ) SI_UNIT ( $, .STERADIAN. ) SOLID_ANGLE_UNIT ( ) );
#5493 = EDGE_CURVE ( 'NONE', #2347, #13326, #5713, .T. ) ;
#5494 = DIRECTION ( 'NONE',  ( -0.000000000000000000, -1.000000000000000000, -0.000000000000000000 ) ) ;
#5495 = B_SPLINE_CURVE_WITH_KNOTS ( 'NONE', 3,
 ( #12445, #5043, #6285, #2020 ),
 .UNSPECIFIED., .F., .F.,
 ( 4, 4 ),
 ( 0.000000000000000000, 0.5855695330273008592 ),
 .UNSPECIFIED. ) ;
#5496 = DIRECTION ( 'NONE',  ( -0.000000000000000000, -1.000000000000000000, 0.000000000000000000 ) ) ;
#5497 = CARTESIAN_POINT ( 'NONE',  ( -7.155006492985575228, 9.000000000000000000, -1.740452503570284915 ) ) ;
#5498 = DIRECTION ( 'NONE',  ( 0.000000000000000000, 1.000000000000000000, -0.000000000000000000 ) ) ;
#5499 = CARTESIAN_POINT ( 'NONE',  ( 5.741477348071313713, 3.000000000000000000, -13.86115248177180703 ) ) ;
#5500 = VERTEX_POINT ( 'NONE', #11184 ) ;
#5501 = DIRECTION ( 'NONE',  ( -0.000000000000000000, -1.000000000000000000, -0.000000000000000000 ) ) ;
#5502 = VERTEX_POINT ( 'NONE', #1753 ) ;
#5503 = ORIENTED_EDGE ( 'NONE', *, *, #12770, .T. ) ;
#5504 = VERTEX_POINT ( 'NONE', #4636 ) ;
#5505 = DIRECTION ( 'NONE',  ( 0.000000000000000000, 0.000000000000000000, 1.000000000000000000 ) ) ;
#5506 = EDGE_CURVE ( 'NONE', #1651, #6481, #3478, .T. ) ;
#5507 = ORIENTED_EDGE ( 'NONE', *, *, #935, .F. ) ;
#5508 = AXIS2_PLACEMENT_3D ( 'NONE', #8845, #3481, #9883 ) ;
#5509 = EDGE_LOOP ( 'NONE', ( #729, #4903, #13508, #6129 ) ) ;
#5510 = VECTOR ( 'NONE', #2654, 1000.000000000000000 ) ;
#5511 = LINE ( 'NONE', #4283, #1424 ) ;
#5512 = SHAPE_REPRESENTATION_RELATIONSHIP ( 'NONE' , 'NONE' ,  #8376, #10000 ) ;
#5513 = EDGE_CURVE ( 'NONE', #464, #641, #587, .T. ) ;
#5514 = CARTESIAN_POINT ( 'NONE',  ( -12.68816982652953840, 3.000000000000000000, -2.830255545554093644 ) ) ;
#5515 = CARTESIAN_POINT ( 'NONE',  ( -12.40347894490204972, 3.000000000000000000, 3.892776652129660064 ) ) ;
#5516 = DIRECTION ( 'NONE',  ( 0.000000000000000000, 0.000000000000000000, -1.000000000000000000 ) ) ;
#5517 = CARTESIAN_POINT ( 'NONE',  ( -11.46814821560793440, 0.000000000000000000, 5.731782959214994477 ) ) ;
#5518 = CARTESIAN_POINT ( 'NONE',  ( 10.00000000000000888, 5.000000000000007105, -6.999999999999998224 ) ) ;
#5519 = ORIENTED_EDGE ( 'NONE', *, *, #2119, .T. ) ;
#5520 = AXIS2_PLACEMENT_3D ( 'NONE', #3398, #11672, #7609 ) ;
#5521 = CARTESIAN_POINT ( 'NONE',  ( 0.000000000000000000, 0.000000000000000000, 0.000000000000000000 ) ) ;
#5522 = AXIS2_PLACEMENT_3D ( 'NONE', #13259, #13051, #10015 ) ;
#5523 = AXIS2_PLACEMENT_3D ( 'NONE', #5003, #3961, #12391 ) ;
#5524 = VERTEX_POINT ( 'NONE', #12568 ) ;
#5525 = EDGE_LOOP ( 'NONE', ( #9368, #1166, #6307, #5902 ) ) ;
#5526 = ORIENTED_EDGE ( 'NONE', *, *, #2184, .F. ) ;
#5527 = CARTESIAN_POINT ( 'NONE',  ( 8.373678438139048552, 9.000000000000000000, 1.459968977288628844 ) ) ;
#5528 = DIRECTION ( 'NONE',  ( -0.000000000000000000, -1.000000000000000000, -0.000000000000000000 ) ) ;
#5529 = VECTOR ( 'NONE', #6697, 1000.000000000000000 ) ;
#5530 = APPLICATION_PROTOCOL_DEFINITION ( 'draft international standard', 'automotive_design', 1998, #3509 ) ;
#5531 = DIRECTION ( 'NONE',  ( 0.000000000000000000, 0.000000000000000000, 1.000000000000000000 ) ) ;
#5532 = DIRECTION ( 'NONE',  ( 0.000000000000000000, 1.000000000000000000, -0.000000000000000000 ) ) ;
#5533 = CARTESIAN_POINT ( 'NONE',  ( 8.430890348300625448, 0.000000000000000000, 11.48836750521723893 ) ) ;
#5534 = CYLINDRICAL_SURFACE ( 'NONE', #3123, 1.500000000000001332 ) ;
#5535 = VERTEX_POINT ( 'NONE', #8343 ) ;
#5536 = EDGE_CURVE ( 'NONE', #5689, #3986, #9014, .T. ) ;
#5537 = CLOSED_SHELL ( 'NONE', ( #1381, #1946, #6817, #4063, #8678, #5745, #9945, #3627, #9611, #12754 ) ) ;
#5538 = ORIENTED_EDGE ( 'NONE', *, *, #1122, .T. ) ;
#5539 = CIRCLE ( 'NONE', #12386, 3.000000000000002665 ) ;
#5540 = CARTESIAN_POINT ( 'NONE',  ( 5.452638258930520010, 3.000000000000000000, -13.97385902380752754 ) ) ;
#5541 = B_SPLINE_SURFACE_WITH_KNOTS ( 'NONE', 3, 1, ( 
 ( #12107, #2456 ),
 ( #6727, #8921 ),
 ( #9958, #10928 ),
 ( #6938, #11970 ) ),
 .UNSPECIFIED., .F., .F., .F.,
 ( 4, 4 ),
 ( 2, 2 ),
 ( 0.1547128134717859205, 0.7774895956119340923 ),
 ( 0.000000000000000000, 1.000000000000000000 ),
 .UNSPECIFIED. ) ;
#5542 = ORIENTED_EDGE ( 'NONE', *, *, #7513, .F. ) ;
#5543 = CARTESIAN_POINT ( 'NONE',  ( 6.000000000000008882, 0.000000000000000000, 28.50000000000000000 ) ) ;
#5544 = APPLICATION_CONTEXT ( 'automotive_design' ) ;
#5545 = CYLINDRICAL_SURFACE ( 'NONE', #12330, 5.486375544325371223 ) ;
#5546 = CIRCLE ( 'NONE', #5329, 1.500000000000000444 ) ;
#5547 = CARTESIAN_POINT ( 'NONE',  ( -12.07794044664754018, 3.000000000000000000, -0.5398653231797256868 ) ) ;
#5548 = VECTOR ( 'NONE', #2288, 1000.000000000000000 ) ;
#5549 = CIRCLE ( 'NONE', #4672, 14.25000000000000178 ) ;
#5550 = CARTESIAN_POINT ( 'NONE',  ( 0.1834774187694905023, 3.000000000000000000, -13.00394734430440025 ) ) ;
#5551 = CARTESIAN_POINT ( 'NONE',  ( -11.46814821560793440, 3.000000000000000000, 5.731782959214994477 ) ) ;
#5552 = B_SPLINE_CURVE_WITH_KNOTS ( 'NONE', 2,
 ( #9305, #2078, #11377 ),
 .UNSPECIFIED., .F., .F.,
 ( 3, 3 ),
 ( 0.000000000000000000, 0.02941149433826504428 ),
 .UNSPECIFIED. ) ;
#5553 = CARTESIAN_POINT ( 'NONE',  ( -10.72973591378220348, 0.000000000000000000, 5.571433138827830867 ) ) ;
#5554 = DIRECTION ( 'NONE',  ( 0.000000000000000000, 0.000000000000000000, 1.000000000000000000 ) ) ;
#5555 = EDGE_CURVE ( 'NONE', #1728, #13138, #11553, .T. ) ;
#5556 = CARTESIAN_POINT ( 'NONE',  ( -8.180229652970899323, 0.000000000000000000, -11.90209577080756276 ) ) ;
#5557 = VERTEX_POINT ( 'NONE', #12302 ) ;
#5558 = ORIENTED_EDGE ( 'NONE', *, *, #4646, .F. ) ;
#5559 = EDGE_LOOP ( 'NONE', ( #10906, #7633, #8090, #12174 ) ) ;
#5560 = ORIENTED_EDGE ( 'NONE', *, *, #2619, .F. ) ;
#5561 = DIRECTION ( 'NONE',  ( -0.000000000000000000, -1.000000000000000000, -0.000000000000000000 ) ) ;
#5562 = EDGE_CURVE ( 'NONE', #1090, #12859, #8359, .T. ) ;
#5563 = ORIENTED_EDGE ( 'NONE', *, *, #5581, .T. ) ;
#5564 = LINE ( 'NONE', #4538, #13190 ) ;
#5565 = CARTESIAN_POINT ( 'NONE',  ( 6.736042615721505200, 9.000000000000000000, 5.184180733653466433 ) ) ;
#5566 = VECTOR ( 'NONE', #4521, 1000.000000000000227 ) ;
#5567 = CARTESIAN_POINT ( 'NONE',  ( -10.18979803820068675, 3.000000000000000000, 6.506620931068438196 ) ) ;
#5568 = PRODUCT ( 'gripper', 'gripper', '', ( #2336 ) ) ;
#5569 = CIRCLE ( 'NONE', #13502, 1.000000000000000888 ) ;
#5570 = AXIS2_PLACEMENT_3D ( 'NONE', #815, #12471, #2801 ) ;
#5571 = EDGE_CURVE ( 'NONE', #9479, #3134, #6167, .T. ) ;
#5572 = CARTESIAN_POINT ( 'NONE',  ( -11.80612203322752585, 0.000000000000000000, 2.604531154829235362 ) ) ;
#5573 = CARTESIAN_POINT ( 'NONE',  ( 11.65525440103098731, 3.000000000000000000, 2.142386537870793362 ) ) ;
#5574 = ORIENTED_EDGE ( 'NONE', *, *, #6917, .T. ) ;
#5575 = DIRECTION ( 'NONE',  ( -0.000000000000000000, -1.000000000000000000, -0.000000000000000000 ) ) ;
#5576 = EDGE_LOOP ( 'NONE', ( #9909, #11467, #7729, #9598 ) ) ;
#5577 = ORIENTED_EDGE ( 'NONE', *, *, #2731, .F. ) ;
#5578 = UNCERTAINTY_MEASURE_WITH_UNIT (LENGTH_MEASURE( 1.000000000000000082E-05 ), #4339, 'distance_accuracy_value', 'NONE');
#5579 = ORIENTED_EDGE ( 'NONE', *, *, #12489, .T. ) ;
#5580 = DIRECTION ( 'NONE',  ( 0.000000000000000000, 0.000000000000000000, 1.000000000000000000 ) ) ;
#5581 = EDGE_CURVE ( 'NONE', #4662, #5132, #12342, .T. ) ;
#5582 = ORIENTED_EDGE ( 'NONE', *, *, #10121, .F. ) ;
#5583 = CIRCLE ( 'NONE', #13070, 5.000000000000000000 ) ;
#5584 = ORIENTED_EDGE ( 'NONE', *, *, #9428, .T. ) ;
#5585 = CARTESIAN_POINT ( 'NONE',  ( 12.00000000000000711, 5.000000000000000000, -6.999999999999999112 ) ) ;
#5586 = CARTESIAN_POINT ( 'NONE',  ( 2.546103534247748712, 3.000000000000000000, -12.55526518755974585 ) ) ;
#5587 = DIRECTION ( 'NONE',  ( 0.000000000000000000, 1.000000000000000000, 0.000000000000000000 ) ) ;
#5588 = CARTESIAN_POINT ( 'NONE',  ( 2.631756770590782057, 0.000000000000000000, -14.20034848914875347 ) ) ;
#5589 = ADVANCED_FACE ( 'NONE', ( #4089 ), #3329, .F. ) ;
#5590 = DIRECTION ( 'NONE',  ( 0.000000000000000000, 0.000000000000000000, -1.000000000000000000 ) ) ;
#5591 = B_SPLINE_CURVE_WITH_KNOTS ( 'NONE', 3,
 ( #10557, #8540, #11525, #6282 ),
 .UNSPECIFIED., .F., .F.,
 ( 4, 4 ),
 ( 0.000000000000000000, 0.5855695330273008592 ),
 .UNSPECIFIED. ) ;
#5592 = EDGE_CURVE ( 'NONE', #2583, #12211, #4175, .T. ) ;
#5593 = CARTESIAN_POINT ( 'NONE',  ( -4.334442004268530546, 9.000000000000000000, 7.311813216407585081 ) ) ;
#5594 = EDGE_LOOP ( 'NONE', ( #9371, #13542, #11744, #12224 ) ) ;
#5595 = DIRECTION ( 'NONE',  ( 0.000000000000000000, 1.000000000000000000, 0.000000000000000000 ) ) ;
#5596 = AXIS2_PLACEMENT_3D ( 'NONE', #12798, #2185, #2250 ) ;
#5597 = ORIENTED_EDGE ( 'NONE', *, *, #12187, .F. ) ;
#5598 = CIRCLE ( 'NONE', #5172, 1.500000000000000222 ) ;
#5599 = VERTEX_POINT ( 'NONE', #12511 ) ;
#5600 = ORIENTED_EDGE ( 'NONE', *, *, #4891, .T. ) ;
#5601 = CARTESIAN_POINT ( 'NONE',  ( 6.951477219042924816, 9.000000000000000000, 3.842108769784387423 ) ) ;
#5602 = AXIS2_PLACEMENT_3D ( 'NONE', #2309, #8426, #2168 ) ;
#5603 = AXIS2_PLACEMENT_3D ( 'NONE', #6497, #1260, #371 ) ;
#5604 = CARTESIAN_POINT ( 'NONE',  ( 3.647470871583629926, 3.000000000000000000, -11.52666717836884125 ) ) ;
#5605 = CONTEXT_DEPENDENT_SHAPE_REPRESENTATION ( #4850, #3595 ) ;
#5606 = CARTESIAN_POINT ( 'NONE',  ( 6.749972395921142621, 0.000000000000000000, -0.01930425607464666612 ) ) ;
#5607 = EDGE_CURVE ( 'NONE', #1734, #2852, #5940, .T. ) ;
#5608 = CARTESIAN_POINT ( 'NONE',  ( -9.065441275458884007, 3.000000000000000000, -9.324917484779556176 ) ) ;
#5609 = CARTESIAN_POINT ( 'NONE',  ( 6.553553527263006551, 1.734723475976807094E-15, 1.616612558808879774 ) ) ;
#5610 = EDGE_CURVE ( 'NONE', #10338, #688, #7259, .T. ) ;
#5611 = DIRECTION ( 'NONE',  ( 0.000000000000000000, 1.000000000000000000, -0.000000000000000000 ) ) ;
#5612 = VERTEX_POINT ( 'NONE', #2023 ) ;
#5613 = VECTOR ( 'NONE', #6489, 1000.000000000000000 ) ;
#5614 = AXIS2_PLACEMENT_3D ( 'NONE', #6879, #5985, #7778 ) ;
#5615 = VERTEX_POINT ( 'NONE', #11255 ) ;
#5616 = CARTESIAN_POINT ( 'NONE',  ( 41.29994854050690378, 3.000000000000000000, -6.141175130212632283 ) ) ;
#5617 = ORIENTED_EDGE ( 'NONE', *, *, #6158, .T. ) ;
#5618 = LINE ( 'NONE', #11826, #2062 ) ;
#5619 = FACE_OUTER_BOUND ( 'NONE', #7273, .T. ) ;
#5620 = EDGE_CURVE ( 'NONE', #10439, #597, #1767, .T. ) ;
#5621 = CARTESIAN_POINT ( 'NONE',  ( 8.208497377870827449, 0.000000000000000000, -8.550000000000002487 ) ) ;
#5622 = CARTESIAN_POINT ( 'NONE',  ( -12.07793442604884682, 0.000000000000000000, 0.5400000000005513723 ) ) ;
#5623 = CARTESIAN_POINT ( 'NONE',  ( 5.280889752749253319, 9.000000000000000000, -6.660495733750448011 ) ) ;
#5624 = CARTESIAN_POINT ( 'NONE',  ( -12.08646469655240097, 3.000000000000000000, -8.883544964651921561 ) ) ;
#5625 = DIRECTION ( 'NONE',  ( 0.000000000000000000, 0.000000000000000000, 1.000000000000000000 ) ) ;
#5626 = DIRECTION ( 'NONE',  ( -0.000000000000000000, -1.000000000000000000, -0.000000000000000000 ) ) ;
#5627 = EDGE_LOOP ( 'NONE', ( #9216, #9100, #9438, #9271 ) ) ;
#5628 = EDGE_LOOP ( 'NONE', ( #13163, #8419, #5710, #575 ) ) ;
#5629 = ORIENTED_EDGE ( 'NONE', *, *, #2484, .F. ) ;
#5630 = ORIENTED_EDGE ( 'NONE', *, *, #6934, .T. ) ;
#5631 = DIRECTION ( 'NONE',  ( 0.000000000000000000, 0.000000000000000000, 1.000000000000000000 ) ) ;
#5632 = ORIENTED_EDGE ( 'NONE', *, *, #4128, .F. ) ;
#5633 = EDGE_CURVE ( 'NONE', #8226, #5615, #10225, .T. ) ;
#5634 = CYLINDRICAL_SURFACE ( 'NONE', #10328, 6.750000000000000888 ) ;
#5635 = ADVANCED_FACE ( 'NONE', ( #9180 ), #13394, .F. ) ;
#5636 = EDGE_CURVE ( 'NONE', #1237, #10281, #1551, .T. ) ;
#5637 = DIRECTION ( 'NONE',  ( 0.000000000000000000, 0.000000000000000000, 1.000000000000000000 ) ) ;
#5638 = CARTESIAN_POINT ( 'NONE',  ( 5.733772933379474246, 3.000000000000000000, -13.04554897075799502 ) ) ;
#5639 = CARTESIAN_POINT ( 'NONE',  ( 8.482622935103764306, 3.000000000000000000, -9.600126836553261711 ) ) ;
#5640 = B_SPLINE_CURVE_WITH_KNOTS ( 'NONE', 3,
 ( #5076, #8169, #12401, #2945 ),
 .UNSPECIFIED., .F., .F.,
 ( 4, 4 ),
 ( 0.000000000000000000, 0.5855695330273008592 ),
 .UNSPECIFIED. ) ;
#5641 = LINE ( 'NONE', #281, #7600 ) ;
#5642 = VERTEX_POINT ( 'NONE', #994 ) ;
#5643 = CYLINDRICAL_SURFACE ( 'NONE', #11956, 1.500000000000000666 ) ;
#5644 = ORIENTED_EDGE ( 'NONE', *, *, #224, .F. ) ;
#5645 = ORIENTED_EDGE ( 'NONE', *, *, #1638, .T. ) ;
#5646 = DIRECTION ( 'NONE',  ( -0.000000000000000000, -1.000000000000000000, -0.000000000000000000 ) ) ;
#5647 = ORIENTED_EDGE ( 'NONE', *, *, #1207, .F. ) ;
#5648 = EDGE_CURVE ( 'NONE', #3799, #6616, #6148, .T. ) ;
#5649 = ORIENTED_EDGE ( 'NONE', *, *, #7105, .F. ) ;
#5650 = EDGE_CURVE ( 'NONE', #1736, #447, #2991, .T. ) ;
#5651 = CARTESIAN_POINT ( 'NONE',  ( -13.82336506795094522, 0.000000000000000000, -0.6724118135761603110 ) ) ;
#5652 = CARTESIAN_POINT ( 'NONE',  ( 54.70014691233865989, 3.000000000000000000, -3.785783530882224746 ) ) ;
#5653 = CARTESIAN_POINT ( 'NONE',  ( 0.9098489087730803337, 0.000000000000000000, 7.307220250892556557 ) ) ;
#5654 = EDGE_CURVE ( 'NONE', #12265, #4927, #3291, .T. ) ;
#5655 = DIRECTION ( 'NONE',  ( -0.000000000000000000, -1.000000000000000000, -0.000000000000000000 ) ) ;
#5656 = EDGE_CURVE ( 'NONE', #11262, #12351, #12215, .T. ) ;
#5657 = CARTESIAN_POINT ( 'NONE',  ( -12.68816982652953840, 0.000000000000000000, -2.830255545554093644 ) ) ;
#5658 = CARTESIAN_POINT ( 'NONE',  ( 31.00000000000000000, 0.000000000000000000, -4.000000001073670930 ) ) ;
#5659 = ORIENTED_EDGE ( 'NONE', *, *, #9280, .F. ) ;
#5660 = LINE ( 'NONE', #3319, #12823 ) ;
#5661 = B_SPLINE_SURFACE_WITH_KNOTS ( 'NONE', 3, 1, ( 
 ( #6652, #11132 ),
 ( #3477, #9818 ),
 ( #10026, #8979 ),
 ( #13193, #1702 ) ),
 .UNSPECIFIED., .F., .F., .F.,
 ( 4, 4 ),
 ( 2, 2 ),
 ( 0.4545418633443863987, 0.4839599404020549223 ),
 ( 0.000000000000000000, 1.000000000000000000 ),
 .UNSPECIFIED. ) ;
#5662 = ORIENTED_EDGE ( 'NONE', *, *, #12086, .F. ) ;
#5663 = ORIENTED_EDGE ( 'NONE', *, *, #3906, .T. ) ;
#5664 = EDGE_LOOP ( 'NONE', ( #7033, #2609, #3630, #4185 ) ) ;
#5665 = EDGE_CURVE ( 'NONE', #9614, #12211, #9680, .T. ) ;
#5666 = CARTESIAN_POINT ( 'NONE',  ( 13.27898586450067420, 3.000000000000000000, 5.170206418547648397 ) ) ;
#5667 = DIRECTION ( 'NONE',  ( 0.000000000000000000, 0.000000000000000000, 1.000000000000000000 ) ) ;
#5668 = PLANE ( 'NONE',  #7277 ) ;
#5669 = CONTEXT_DEPENDENT_SHAPE_REPRESENTATION ( #6969, #8640 ) ;
#5670 = CARTESIAN_POINT ( 'NONE',  ( -7.751044794789887504, 0.000000000000000000, 1.733822342365972879 ) ) ;
#5671 = DIRECTION ( 'NONE',  ( 0.000000000000000000, 1.000000000000000000, 0.000000000000000000 ) ) ;
#5672 = CARTESIAN_POINT ( 'NONE',  ( 30.73000000000000043, 3.000000000000000000, -5.500000000000003553 ) ) ;
#5673 = CARTESIAN_POINT ( 'NONE',  ( 0.7868956173019259204, 0.000000000000000000, 7.903520140620750034 ) ) ;
#5674 = ORIENTED_EDGE ( 'NONE', *, *, #7176, .F. ) ;
#5675 = VERTEX_POINT ( 'NONE', #4677 ) ;
#5676 = ADVANCED_FACE ( 'NONE', ( #11731, #12703, #1508 ), #8863, .T. ) ;
#5677 = EDGE_CURVE ( 'NONE', #2261, #3196, #6441, .T. ) ;
#5678 = ORIENTED_EDGE ( 'NONE', *, *, #181, .T. ) ;
#5679 = LINE ( 'NONE', #7879, #12843 ) ;
#5680 = PRODUCT_DEFINITION_SHAPE ( 'NONE', 'NONE',  #13601 ) ;
#5681 = CARTESIAN_POINT ( 'NONE',  ( 29.39270799701850123, 3.000000000000000000, -0.3930766723116408401 ) ) ;
#5682 = FACE_OUTER_BOUND ( 'NONE', #11111, .T. ) ;
#5683 = CARTESIAN_POINT ( 'NONE',  ( 4.164551629694410728, 0.000000000000000000, -6.072874324029720050 ) ) ;
#5684 = CARTESIAN_POINT ( 'NONE',  ( 0.000000000000000000, 3.000000000000000000, 0.000000000000000000 ) ) ;
#5685 = CARTESIAN_POINT ( 'NONE',  ( 31.00000000000000000, 3.000000000000000000, 0.000000000000000000 ) ) ;
#5686 = DIRECTION ( 'NONE',  ( 0.000000000000000000, 0.000000000000000000, -1.000000000000000000 ) ) ;
#5687 = CARTESIAN_POINT ( 'NONE',  ( 8.914835885878220623, 0.000000000000000000, -11.11702303352196708 ) ) ;
#5688 = ORIENTED_EDGE ( 'NONE', *, *, #5019, .F. ) ;
#5689 = VERTEX_POINT ( 'NONE', #8410 ) ;
#5690 = ORIENTED_EDGE ( 'NONE', *, *, #2196, .F. ) ;
#5691 = ORIENTED_EDGE ( 'NONE', *, *, #8708, .T. ) ;
#5692 = CARTESIAN_POINT ( 'NONE',  ( 11.70905276178455878, 3.000000000000000000, -9.375397774054460953 ) ) ;
#5694 = VERTEX_POINT ( 'NONE', #2604 ) ;
#5693 = B_SPLINE_CURVE_WITH_KNOTS ( 'NONE', 3,
 ( #7464, #7530, #10904, #11738 ),
 .UNSPECIFIED., .F., .F.,
 ( 4, 4 ),
 ( 0.1547128134717859205, 1.000000000000000000 ),
 .UNSPECIFIED. ) ;
#5695 = AXIS2_PLACEMENT_3D ( 'NONE', #13144, #4465, #10939 ) ;
#5696 = CARTESIAN_POINT ( 'NONE',  ( 11.14709020439929787, 3.000000000000000000, 7.712570079660892475 ) ) ;
#5697 = DIRECTION ( 'NONE',  ( 0.000000000000000000, 1.000000000000000000, 0.000000000000000000 ) ) ;
#5698 = CARTESIAN_POINT ( 'NONE',  ( -2.604399508763953985, 3.000000000000000000, 11.80615107470197778 ) ) ;
#5699 = CARTESIAN_POINT ( 'NONE',  ( 8.252687871541629860, 0.000000000000000000, 31.00000000000000000 ) ) ;
#5700 = DIRECTION ( 'NONE',  ( -0.000000000000000000, -1.000000000000000000, -0.000000000000000000 ) ) ;
#5701 = CYLINDRICAL_SURFACE ( 'NONE', #12229, 12.08999999999737440 ) ;
#5702 = ORIENTED_EDGE ( 'NONE', *, *, #1991, .T. ) ;
#5703 = FACE_OUTER_BOUND ( 'NONE', #2498, .T. ) ;
#5704 = VERTEX_POINT ( 'NONE', #12637 ) ;
#5705 = EDGE_CURVE ( 'NONE', #11639, #5259, #4357, .T. ) ;
#5706 = PRODUCT_DEFINITION ( 'UNKNOWN', '', #13112, #11920 ) ;
#5707 = EDGE_LOOP ( 'NONE', ( #12309, #7371, #4777, #9492 ) ) ;
#5708 = LINE ( 'NONE', #7516, #5766 ) ;
#5709 = ORIENTED_EDGE ( 'NONE', *, *, #3844, .T. ) ;
#5710 = ORIENTED_EDGE ( 'NONE', *, *, #6023, .F. ) ;
#5711 = CARTESIAN_POINT ( 'NONE',  ( 5.452638258930520010, 0.000000000000000000, -13.97385902380752754 ) ) ;
#5712 = DIRECTION ( 'NONE',  ( 1.000000000000000000, 0.000000000000000000, 0.000000000000000000 ) ) ;
#5713 = CIRCLE ( 'NONE', #6605, 14.25000000000000355 ) ;
#5714 = CARTESIAN_POINT ( 'NONE',  ( -14.39763212228013955, 0.000000000000000000, -1.133238802859595884 ) ) ;
#5715 = AXIS2_PLACEMENT_3D ( 'NONE', #6333, #213, #1100 ) ;
#5716 = DIRECTION ( 'NONE',  ( 0.3802634127332040759, 0.000000000000000000, 0.9248782281665499649 ) ) ;
#5717 = CARTESIAN_POINT ( 'NONE',  ( 51.38094353598858532, 0.000000000000000000, -3.436371243710653722 ) ) ;
#5718 = FACE_OUTER_BOUND ( 'NONE', #7463, .T. ) ;
#5719 = EDGE_LOOP ( 'NONE', ( #1962, #12911, #3222, #10099 ) ) ;
#5720 = CARTESIAN_POINT ( 'NONE',  ( 0.000000000000000000, 0.09999999999999982514, -3.500000000000000888 ) ) ;
#5721 = EDGE_CURVE ( 'NONE', #3089, #9203, #8150, .T. ) ;
#5722 = ORIENTED_EDGE ( 'NONE', *, *, #10382, .T. ) ;
#5723 = EDGE_CURVE ( 'NONE', #3444, #13127, #6800, .T. ) ;
#5724 = ORIENTED_EDGE ( 'NONE', *, *, #12506, .T. ) ;
#5725 = CIRCLE ( 'NONE', #3969, 3.000000000000000444 ) ;
#5726 = B_SPLINE_SURFACE_WITH_KNOTS ( 'NONE', 3, 1, ( 
 ( #8799, #8740 ),
 ( #483, #1517 ),
 ( #4687, #2352 ),
 ( #12955, #4413 ) ),
 .UNSPECIFIED., .F., .F., .F.,
 ( 4, 4 ),
 ( 2, 2 ),
 ( 0.09090310649439187207, 0.1203211835519651524 ),
 ( 0.000000000000000000, 1.000000000000000000 ),
 .UNSPECIFIED. ) ;
#5727 = VECTOR ( 'NONE', #7685, 1000.000000000000000 ) ;
#5728 = ORIENTED_EDGE ( 'NONE', *, *, #2731, .T. ) ;
#5729 = EDGE_CURVE ( 'NONE', #4139, #4943, #452, .T. ) ;
#5730 = EDGE_CURVE ( 'NONE', #2610, #12350, #4192, .T. ) ;
#5731 = B_SPLINE_CURVE_WITH_KNOTS ( 'NONE', 2,
 ( #3427, #7639, #11843 ),
 .UNSPECIFIED., .F., .F.,
 ( 3, 3 ),
 ( 0.000000000000000000, 1.000000000000000000 ),
 .UNSPECIFIED. ) ;
#5732 = CYLINDRICAL_SURFACE ( 'NONE', #8006, 1.499999999999999556 ) ;
#5733 = CARTESIAN_POINT ( 'NONE',  ( 3.647470871583629926, 0.000000000000000000, -11.52666717836884125 ) ) ;
#5734 = CARTESIAN_POINT ( 'NONE',  ( -14.08504230442586369, 0.000000000000000000, 2.161962830978784389 ) ) ;
#5735 = CARTESIAN_POINT ( 'NONE',  ( 0.000000000000000000, -8.809142651444723526E-17, 1.600000000000000311 ) ) ;
#5736 = ITEM_DEFINED_TRANSFORMATION ( 'NONE', 'NONE', #12252,  #10007 ) ;
#5737 = CARTESIAN_POINT ( 'NONE',  ( 6.506507307819716424, 0.000000000000000000, -10.18987059060247269 ) ) ;
#5738 = VECTOR ( 'NONE', #7673, 1000.000000000000000 ) ;
#5739 = CYLINDRICAL_SURFACE ( 'NONE', #915, 8.500000000000000000 ) ;
#5740 = DIRECTION ( 'NONE',  ( -0.000000000000000000, -1.000000000000000000, -0.000000000000000000 ) ) ;
#5741 = DIRECTION ( 'NONE',  ( 0.000000000000000000, 0.000000000000000000, -1.000000000000000000 ) ) ;
#5742 = ADVANCED_FACE ( 'NONE', ( #7396 ), #10053, .F. ) ;
#5743 = ORIENTED_EDGE ( 'NONE', *, *, #1447, .F. ) ;
#5744 = EDGE_LOOP ( 'NONE', ( #7347, #3102, #6760, #3333, #4460, #3055, #372, #6429, #10098, #4187, #9785, #12952, #11869, #13203, #2299, #292, #1264, #3903, #11158, #13156, #6790, #13358, #5709, #9887, #10508, #2700, #9441 ) ) ;
#5745 = ADVANCED_FACE ( 'NONE', ( #1121 ), #10944, .F. ) ;
#5746 = AXIS2_PLACEMENT_3D ( 'NONE', #3663, #2776, #2704 ) ;
#5747 = EDGE_CURVE ( 'NONE', #3799, #2502, #2006, .T. ) ;
#5748 = ORIENTED_EDGE ( 'NONE', *, *, #1521, .F. ) ;
#5749 = CARTESIAN_POINT ( 'NONE',  ( 5.733772933379541747, 0.000000000000000000, 13.04554897075796482 ) ) ;
#5750 = DIRECTION ( 'NONE',  ( -0.000000000000000000, -1.000000000000000000, -0.000000000000000000 ) ) ;
#5751 = FACE_OUTER_BOUND ( 'NONE', #9189, .T. ) ;
#5752 = LINE ( 'NONE', #12931, #3306 ) ;
#5753 = PLANE ( 'NONE',  #8791 ) ;
#5754 = CARTESIAN_POINT ( 'NONE',  ( 6.951477219042924816, 0.000000000000000000, 3.842108769784387423 ) ) ;
#5755 = AXIS2_PLACEMENT_3D ( 'NONE', #2237, #2174, #13294 ) ;
#5756 = ADVANCED_FACE ( 'NONE', ( #8482 ), #7959, .F. ) ;
#5757 = CARTESIAN_POINT ( 'NONE',  ( 0.000000000000000000, 0.000000000000000000, 0.000000000000000000 ) ) ;
#5758 = EDGE_CURVE ( 'NONE', #1419, #1362, #12270, .T. ) ;
#5759 = CARTESIAN_POINT ( 'NONE',  ( 0.000000000000000000, 9.000000000000000000, 0.000000000000000000 ) ) ;
#5760 = ORIENTED_EDGE ( 'NONE', *, *, #3722, .F. ) ;
#5761 = EDGE_LOOP ( 'NONE', ( #166, #1436, #7828, #3334 ) ) ;
#5762 = ORIENTED_EDGE ( 'NONE', *, *, #7710, .F. ) ;
#5763 = FACE_OUTER_BOUND ( 'NONE', #9983, .T. ) ;
#5764 = AXIS2_PLACEMENT_3D ( 'NONE', #4968, #698, #8066 ) ;
#5765 = ORIENTED_EDGE ( 'NONE', *, *, #13406, .F. ) ;
#5766 = VECTOR ( 'NONE', #289, 1000.000000000000227 ) ;
#5767 = VECTOR ( 'NONE', #12373, 1000.000000000000000 ) ;
#5768 = VECTOR ( 'NONE', #3947, 1000.000000000000000 ) ;
#5769 = CARTESIAN_POINT ( 'NONE',  ( -11.11702303352192445, 3.000000000000000000, 8.914835885878272137 ) ) ;
#5770 = DIRECTION ( 'NONE',  ( -2.891205793294677833E-16, 0.000000000000000000, 1.000000000000000000 ) ) ;
#5771 = B_SPLINE_SURFACE_WITH_KNOTS ( 'NONE', 3, 1, ( 
 ( #6125, #10188 ),
 ( #9289, #9217 ),
 ( #13567, #8256 ),
 ( #766, #5162 ) ),
 .UNSPECIFIED., .F., .F., .F.,
 ( 4, 4 ),
 ( 2, 2 ),
 ( 0.1276832474596250877, 1.000000000000000000 ),
 ( 0.000000000000000000, 1.000000000000000000 ),
 .UNSPECIFIED. ) ;
#5772 = CARTESIAN_POINT ( 'NONE',  ( 0.000000000000000000, 9.000000000000000000, 0.000000000000000000 ) ) ;
#5773 = DIRECTION ( 'NONE',  ( 0.000000000000000000, 0.000000000000000000, 1.000000000000000000 ) ) ;
#5774 = DIRECTION ( 'NONE',  ( -1.000000000000000000, 0.000000000000000000, 1.261435711112880913E-16 ) ) ;
#5775 = FACE_OUTER_BOUND ( 'NONE', #3138, .T. ) ;
#5776 = FACE_OUTER_BOUND ( 'NONE', #398, .T. ) ;
#5777 = VERTEX_POINT ( 'NONE', #9151 ) ;
#5778 = AXIS2_PLACEMENT_3D ( 'NONE', #3558, #4461, #1236 ) ;
#5779 = AXIS2_PLACEMENT_3D ( 'NONE', #8773, #7819, #12993 ) ;
#5780 = VECTOR ( 'NONE', #4756, 1000.000000000000000 ) ;
#5781 = EDGE_LOOP ( 'NONE', ( #10707, #9191, #10325, #2192 ) ) ;
#5782 = ORIENTED_EDGE ( 'NONE', *, *, #11317, .T. ) ;
#5783 = CARTESIAN_POINT ( 'NONE',  ( 7.712570079660896916, 0.000000000000000000, -11.14709020439929432 ) ) ;
#5784 = EDGE_LOOP ( 'NONE', ( #5821, #8382, #5040, #7788 ) ) ;
#5785 = VERTEX_POINT ( 'NONE', #12410 ) ;
#5786 = CARTESIAN_POINT ( 'NONE',  ( 1.127406311874972422, 9.000000000000000000, -7.862174656777307646 ) ) ;
#5787 = VECTOR ( 'NONE', #2932, 1000.000000000000000 ) ;
#5788 = B_SPLINE_CURVE_WITH_KNOTS ( 'NONE', 3,
 ( #185, #8559, #2042, #11476 ),
 .UNSPECIFIED., .F., .F.,
 ( 4, 4 ),
 ( 0.000000000000000000, 0.8452273900860258760 ),
 .UNSPECIFIED. ) ;
#5789 = VECTOR ( 'NONE', #1333, 1000.000000000000000 ) ;
#5790 = CIRCLE ( 'NONE', #9750, 3.000000000000000000 ) ;
#5791 = FACE_OUTER_BOUND ( 'NONE', #8139, .T. ) ;
#5792 = FACE_OUTER_BOUND ( 'NONE', #5628, .T. ) ;
#5793 = EDGE_CURVE ( 'NONE', #75, #6767, #1337, .T. ) ;
#5794 = DIRECTION ( 'NONE',  ( 0.000000000000000000, 1.000000000000000000, 0.000000000000000000 ) ) ;
#5795 = DIRECTION ( 'NONE',  ( 0.000000000000000000, 1.000000000000000000, -0.000000000000000000 ) ) ;
#5796 = DIRECTION ( 'NONE',  ( 0.6204948238377419045, 0.000000000000000000, -0.7842105416216805791 ) ) ;
#5797 = ORIENTED_EDGE ( 'NONE', *, *, #6702, .F. ) ;
#5798 = CARTESIAN_POINT ( 'NONE',  ( -0.4399887592034530392, 9.000000000000000000, 8.488604708182295511 ) ) ;
#5799 = ORIENTED_EDGE ( 'NONE', *, *, #8171, .T. ) ;
#5800 = AXIS2_PLACEMENT_3D ( 'NONE', #3955, #7145, #11407 ) ;
#5801 = VERTEX_POINT ( 'NONE', #7165 ) ;
#5802 = CIRCLE ( 'NONE', #7352, 6.750000000000001776 ) ;
#5803 = VERTEX_POINT ( 'NONE', #618 ) ;
#5804 = CARTESIAN_POINT ( 'NONE',  ( 6.530577460941774603, 9.000000000000000000, 3.402183248810843885 ) ) ;
#5805 = DIRECTION ( 'NONE',  ( 0.000000000000000000, 0.000000000000000000, 1.000000000000000000 ) ) ;
#5806 = EDGE_CURVE ( 'NONE', #11316, #6828, #8997, .T. ) ;
#5807 = CARTESIAN_POINT ( 'NONE',  ( -6.970598036433426792, 0.000000000000000000, -10.97318381393771780 ) ) ;
#5808 = DIRECTION ( 'NONE',  ( -0.000000000000000000, -1.000000000000000000, 0.000000000000000000 ) ) ;
#5809 = EDGE_CURVE ( 'NONE', #2693, #13368, #7020, .T. ) ;
#5810 = CARTESIAN_POINT ( 'NONE',  ( -1.650143266773857142, 3.000000000000000000, -14.90895795148409952 ) ) ;
#5811 = CONTEXT_DEPENDENT_SHAPE_REPRESENTATION ( #11270, #1405 ) ;
#5812 = AXIS2_PLACEMENT_3D ( 'NONE', #8915, #10090, #4793 ) ;
#5813 = DIRECTION ( 'NONE',  ( 0.000000000000000000, 0.000000000000000000, -1.000000000000000000 ) ) ;
#5815 = EDGE_CURVE ( 'NONE', #4598, #13228, #12123, .T. ) ;
#5814 = VECTOR ( 'NONE', #554, 1000.000000000000000 ) ;
#5816 = DIRECTION ( 'NONE',  ( -1.000000000000000000, 3.469446951953610639E-15, 2.602085213965210149E-16 ) ) ;
#5817 = DIRECTION ( 'NONE',  ( -0.000000000000000000, -1.000000000000000000, -0.000000000000000000 ) ) ;
#5818 = CARTESIAN_POINT ( 'NONE',  ( -1.557181465540760534, 0.000000000000000000, -14.16466328168009703 ) ) ;
#5819 = CARTESIAN_POINT ( 'NONE',  ( 5.967832595844252630, 9.000000000000000000, -3.153961652902406154 ) ) ;
#5820 = EDGE_CURVE ( 'NONE', #3324, #13428, #3275, .T. ) ;
#5821 = ORIENTED_EDGE ( 'NONE', *, *, #12017, .F. ) ;
#5822 = ORIENTED_EDGE ( 'NONE', *, *, #5080, .F. ) ;
#5823 = MECHANICAL_DESIGN_GEOMETRIC_PRESENTATION_REPRESENTATION (  '', ( #11764 ), #11108 ) ;
#5824 = AXIS2_PLACEMENT_3D ( 'NONE', #12075, #2767, #13106 ) ;
#5825 = ORIENTED_EDGE ( 'NONE', *, *, #9550, .F. ) ;
#5826 = CARTESIAN_POINT ( 'NONE',  ( -3.533475733155563070, 0.000000000000000000, 7.730753471893976325 ) ) ;
#5827 = PLANE ( 'NONE',  #1859 ) ;
#5828 = EDGE_CURVE ( 'NONE', #9614, #8871, #5077, .T. ) ;
#5829 = CARTESIAN_POINT ( 'NONE',  ( 0.000000000000000000, 9.000000000000000000, 0.000000000000000000 ) ) ;
#5830 = CARTESIAN_POINT ( 'NONE',  ( -14.08504230442586369, 3.000000000000000000, 2.161962830978781724 ) ) ;
#5831 = MECHANICAL_DESIGN_GEOMETRIC_PRESENTATION_REPRESENTATION (  '', ( #11998 ), #7598 ) ;
#5832 = EDGE_CURVE ( 'NONE', #9256, #9763, #2952, .T. ) ;
#5833 = CARTESIAN_POINT ( 'NONE',  ( -7.494008246337227952, 3.000000000000000000, -11.63517940784355886 ) ) ;
#5834 = AXIS2_PLACEMENT_3D ( 'NONE', #11781, #12948, #1178 ) ;
#5835 = EDGE_CURVE ( 'NONE', #4996, #10780, #10182, .T. ) ;
#5836 = DIRECTION ( 'NONE',  ( 0.000000000000000000, 0.000000000000000000, 1.000000000000000000 ) ) ;
#5837 = CARTESIAN_POINT ( 'NONE',  ( -12.98835496148299207, 3.000000000000000000, 0.5501230721524459355 ) ) ;
#5838 = ORIENTED_EDGE ( 'NONE', *, *, #9435, .T. ) ;
#5839 = VERTEX_POINT ( 'NONE', #3908 ) ;
#5840 = ORIENTED_EDGE ( 'NONE', *, *, #6745, .T. ) ;
#5841 = DIRECTION ( 'NONE',  ( 0.000000000000000000, 0.000000000000000000, 1.000000000000000000 ) ) ;
#5842 = ORIENTED_EDGE ( 'NONE', *, *, #1526, .T. ) ;
#5843 =( GEOMETRIC_REPRESENTATION_CONTEXT ( 3 ) GLOBAL_UNCERTAINTY_ASSIGNED_CONTEXT ( ( #12063 ) ) GLOBAL_UNIT_ASSIGNED_CONTEXT ( ( #8067, #11505, #13512 ) ) REPRESENTATION_CONTEXT ( 'NONE', 'WORKASPACE' ) );
#5844 = CARTESIAN_POINT ( 'NONE',  ( -2.604531154829235362, 0.000000000000000000, -11.80612203322752585 ) ) ;
#5845 = DIRECTION ( 'NONE',  ( 1.000000000000000000, 0.000000000000000000, 0.000000000000000000 ) ) ;
#5846 = LINE ( 'NONE', #1507, #12783 ) ;
#5847 = CARTESIAN_POINT ( 'NONE',  ( -6.721397655168936502, 0.000000000000000000, 5.203154193476255074 ) ) ;
#5848 = CARTESIAN_POINT ( 'NONE',  ( 5.985774866078160450, 9.000000000000000000, 3.119775513178307147 ) ) ;
#5849 = CARTESIAN_POINT ( 'NONE',  ( -11.17001009226120445, 0.000000000000000000, -6.660869730750943241 ) ) ;
#5850 = CARTESIAN_POINT ( 'NONE',  ( -2.551540321038929007E-15, 2.000000000000000000, -7.000000000000000000 ) ) ;
#5851 = B_SPLINE_CURVE_WITH_KNOTS ( 'NONE', 3,
 ( #13137, #12935, #8986, #2459 ),
 .UNSPECIFIED., .F., .F.,
 ( 4, 4 ),
 ( 0.1547128134717859205, 0.7774895956119340923 ),
 .UNSPECIFIED. ) ;
#5852 = ORIENTED_EDGE ( 'NONE', *, *, #10574, .F. ) ;
#5853 = ORIENTED_EDGE ( 'NONE', *, *, #1229, .T. ) ;
#5854 = DIRECTION ( 'NONE',  ( -0.000000000000000000, -1.000000000000000000, -0.000000000000000000 ) ) ;
#5855 = ORIENTED_EDGE ( 'NONE', *, *, #11388, .T. ) ;
#5856 = VERTEX_POINT ( 'NONE', #11082 ) ;
#5857 = LINE ( 'NONE', #12280, #2913 ) ;
#5858 = EDGE_LOOP ( 'NONE', ( #7010, #5038, #7099, #8586 ) ) ;
#5859 = CARTESIAN_POINT ( 'NONE',  ( 8.760376775873721655, 0.000000000000000000, -10.34346111134700585 ) ) ;
#5860 = ADVANCED_FACE ( 'NONE', ( #4750 ), #11152, .T. ) ;
#5861 = ORIENTED_EDGE ( 'NONE', *, *, #11561, .T. ) ;
#5862 = EDGE_CURVE ( 'NONE', #12859, #1887, #2984, .T. ) ;
#5863 = FACE_OUTER_BOUND ( 'NONE', #10171, .T. ) ;
#5864 =( LENGTH_UNIT ( ) NAMED_UNIT ( * ) SI_UNIT ( .MILLI., .METRE. ) );
#5865 = DIRECTION ( 'NONE',  ( -0.6291930273682727615, 0.000000000000000000, 0.7772490812546181127 ) ) ;
#5866 = CARTESIAN_POINT ( 'NONE',  ( 5.051606143860416509, 9.000000000000000000, 4.477027514692274224 ) ) ;
#5867 = CARTESIAN_POINT ( 'NONE',  ( -12.78643498603817896, 3.000000000000000000, 0.7901945867173603144 ) ) ;
#5868 = CARTESIAN_POINT ( 'NONE',  ( -20.56403552112892896, 0.000000000000000000, -16.70078978407140013 ) ) ;
#5869 = DIRECTION ( 'NONE',  ( 0.000000000000000000, 0.000000000000000000, 1.000000000000000000 ) ) ;
#5870 = EDGE_LOOP ( 'NONE', ( #11821, #3506 ) ) ;
#5871 = DIRECTION ( 'NONE',  ( 0.000000000000000000, 0.000000000000000000, 1.000000000000000000 ) ) ;
#5872 = ORIENTED_EDGE ( 'NONE', *, *, #4482, .F. ) ;
#5873 = ORIENTED_EDGE ( 'NONE', *, *, #6422, .F. ) ;
#5874 = CARTESIAN_POINT ( 'NONE',  ( 7.758214145541979967, -1.694065894508600678E-18, 1.700281702449083054 ) ) ;
#5875 = ORIENTED_EDGE ( 'NONE', *, *, #1879, .F. ) ;
#5876 = B_SPLINE_SURFACE_WITH_KNOTS ( 'NONE', 3, 1, ( 
 ( #3978, #8178 ),
 ( #7898, #10106 ),
 ( #12121, #2671 ),
 ( #1657, #5847 ) ),
 .UNSPECIFIED., .F., .F., .F.,
 ( 4, 4 ),
 ( 2, 2 ),
 ( 0.000000000000000000, 0.8724294488011775650 ),
 ( 0.000000000000000000, 1.000000000000000000 ),
 .UNSPECIFIED. ) ;
#5877 = DIRECTION ( 'NONE',  ( 0.000000000000000000, 1.000000000000000000, -0.000000000000000000 ) ) ;
#5878 = CARTESIAN_POINT ( 'NONE',  ( -12.55526518755974585, 3.000000000000000000, -2.546103534247746047 ) ) ;
#5879 = CARTESIAN_POINT ( 'NONE',  ( -8.158651161643904359, 0.000000000000000000, -8.922136023539605887 ) ) ;
#5880 = CARTESIAN_POINT ( 'NONE',  ( 1.959434878635765477E-16, -8.809142651444723526E-17, -1.600000000000000311 ) ) ;
#5881 = CARTESIAN_POINT ( 'NONE',  ( -1.650143266773857142, 0.000000000000000000, -14.90895795148409952 ) ) ;
#5882 = DIRECTION ( 'NONE',  ( 0.000000000000000000, 0.000000000000000000, 1.000000000000000000 ) ) ;
#5883 = LINE ( 'NONE', #8017, #12774 ) ;
#5884 = DIRECTION ( 'NONE',  ( -0.000000000000000000, -1.000000000000000000, -0.000000000000000000 ) ) ;
#5885 = CARTESIAN_POINT ( 'NONE',  ( -2.161962830978783057, 0.000000000000000000, -14.08504230442586369 ) ) ;
#5886 = DIRECTION ( 'NONE',  ( 0.000000000000000000, 0.000000000000000000, -1.000000000000000000 ) ) ;
#5887 = VERTEX_POINT ( 'NONE', #7089 ) ;
#5888 = ORIENTED_EDGE ( 'NONE', *, *, #3282, .F. ) ;
#5889 = EDGE_CURVE ( 'NONE', #6233, #12697, #9902, .T. ) ;
#5890 = VERTEX_POINT ( 'NONE', #3696 ) ;
#5891 = DIRECTION ( 'NONE',  ( 1.269138026879196405E-16, 0.000000000000000000, 1.000000000000000000 ) ) ;
#5892 = DIRECTION ( 'NONE',  ( 1.000000000000000000, 0.000000000000000000, -0.000000000000000000 ) ) ;
#5893 = CARTESIAN_POINT ( 'NONE',  ( 31.00000000000000000, 0.000000000000000000, -1.073670993220974656E-09 ) ) ;
#5894 = DIRECTION ( 'NONE',  ( -0.000000000000000000, -1.000000000000000000, -0.000000000000000000 ) ) ;
#5895 = CARTESIAN_POINT ( 'NONE',  ( -8.883544964652065445, 3.000000000000000000, -12.08646469655229438 ) ) ;
#5896 = DIRECTION ( 'NONE',  ( 0.000000000000000000, 1.000000000000000000, -0.000000000000000000 ) ) ;
#5897 = CYLINDRICAL_SURFACE ( 'NONE', #11077, 8.499999999999996447 ) ;
#5898 = VERTEX_POINT ( 'NONE', #6954 ) ;
#5899 = ADVANCED_FACE ( 'NONE', ( #9211 ), #5876, .T. ) ;
#5900 = VERTEX_POINT ( 'NONE', #4875 ) ;
#5901 = ADVANCED_FACE ( 'NONE', ( #9072 ), #162, .F. ) ;
#5902 = ORIENTED_EDGE ( 'NONE', *, *, #4912, .T. ) ;
#5903 = LINE ( 'NONE', #545, #6227 ) ;
#5904 = ORIENTED_EDGE ( 'NONE', *, *, #2322, .T. ) ;
#5905 = EDGE_CURVE ( 'NONE', #7779, #4457, #5725, .T. ) ;
#5906 = EDGE_CURVE ( 'NONE', #5900, #9964, #9420, .T. ) ;
#5907 = CYLINDRICAL_SURFACE ( 'NONE', #11870, 12.08999999999737440 ) ;
#5908 = DIRECTION ( 'NONE',  ( 1.000000000000000000, 0.000000000000000000, 0.000000000000000000 ) ) ;
#5909 = DIRECTION ( 'NONE',  ( 0.000000000000000000, 1.000000000000000000, -0.000000000000000000 ) ) ;
#5910 = CARTESIAN_POINT ( 'NONE',  ( 4.690415759823430619, 0.1000000000000000056, -1.399999999999999911 ) ) ;
#5911 = DIRECTION ( 'NONE',  ( 0.000000000000000000, 0.000000000000000000, 1.000000000000000000 ) ) ;
#5912 = CARTESIAN_POINT ( 'NONE',  ( 6.017756925049591921, 3.000000000000000000, -11.52330688609011844 ) ) ;
#5913 = DIRECTION ( 'NONE',  ( 0.000000000000000000, 0.000000000000000000, -1.000000000000000000 ) ) ;
#5914 = ORIENTED_EDGE ( 'NONE', *, *, #1276, .T. ) ;
#5915 = DIRECTION ( 'NONE',  ( -0.000000000000000000, -1.000000000000000000, -0.000000000000000000 ) ) ;
#5916 = EDGE_CURVE ( 'NONE', #9457, #8093, #6380, .T. ) ;
#5917 = VERTEX_POINT ( 'NONE', #12602 ) ;
#5918 = VERTEX_POINT ( 'NONE', #10465 ) ;
#5919 = DIRECTION ( 'NONE',  ( 0.6291930273682743158, 0.000000000000000000, -0.7772490812546168915 ) ) ;
#5920 = ORIENTED_EDGE ( 'NONE', *, *, #12852, .F. ) ;
#5921 = CARTESIAN_POINT ( 'NONE',  ( -13.04554897075795949, 3.000000000000000000, 5.733772933379550629 ) ) ;
#5922 = EDGE_CURVE ( 'NONE', #10329, #11033, #12780, .T. ) ;
#5923 = ORIENTED_EDGE ( 'NONE', *, *, #4595, .F. ) ;
#5924 = DIRECTION ( 'NONE',  ( -0.000000000000000000, -1.000000000000000000, -0.000000000000000000 ) ) ;
#5925 = B_SPLINE_CURVE_WITH_KNOTS ( 'NONE', 3,
 ( #10245, #9056, #7006, #743 ),
 .UNSPECIFIED., .F., .F.,
 ( 4, 4 ),
 ( 0.000000000000000000, 0.8724294488011762327 ),
 .UNSPECIFIED. ) ;
#5926 =( NAMED_UNIT ( * ) PLANE_ANGLE_UNIT ( ) SI_UNIT ( $, .RADIAN. ) );
#5927 = DIRECTION ( 'NONE',  ( -1.000000000000000000, 0.000000000000000000, 0.000000000000000000 ) ) ;
#5928 = CARTESIAN_POINT ( 'NONE',  ( 0.4639228963249704130, 9.000000000000000000, 8.487330295579726069 ) ) ;
#5929 = FACE_OUTER_BOUND ( 'NONE', #10937, .T. ) ;
#5930 = LINE ( 'NONE', #5717, #8166 ) ;
#5931 = DIRECTION ( 'NONE',  ( -0.000000000000000000, -1.000000000000000000, -0.000000000000000000 ) ) ;
#5932 = ORIENTED_EDGE ( 'NONE', *, *, #5021, .F. ) ;
#5933 = DIRECTION ( 'NONE',  ( 0.000000000000000000, 1.000000000000000000, 0.000000000000000000 ) ) ;
#5934 = EDGE_CURVE ( 'NONE', #10050, #9874, #7252, .T. ) ;
#5935 = ORIENTED_EDGE ( 'NONE', *, *, #860, .T. ) ;
#5936 = ADVANCED_FACE ( 'NONE', ( #12730 ), #7628, .F. ) ;
#5937 = ORIENTED_EDGE ( 'NONE', *, *, #9942, .F. ) ;
#5938 = LINE ( 'NONE', #3800, #12817 ) ;
#5939 = EDGE_LOOP ( 'NONE', ( #1438, #5123, #8023, #6357 ) ) ;
#5940 = CIRCLE ( 'NONE', #14, 12.08999999999737263 ) ;
#5941 = CIRCLE ( 'NONE', #3284, 12.08999999999737440 ) ;
#5942 = CARTESIAN_POINT ( 'NONE',  ( 8.771102293099069414, 3.000000000000000000, 10.33484986938308303 ) ) ;
#5943 = CARTESIAN_POINT ( 'NONE',  ( 11.48836750521724070, 3.000000000000000000, -8.430890348300621895 ) ) ;
#5944 = DIRECTION ( 'NONE',  ( 0.9893737785712105604, -0.000000000000000000, -0.1453943818575020863 ) ) ;
#5945 = DIRECTION ( 'NONE',  ( 0.000000000000000000, 1.000000000000000000, -0.000000000000000000 ) ) ;
#5946 = CARTESIAN_POINT ( 'NONE',  ( 3.061616997868383634E-16, 1.000000000000000000, 2.500000000000000444 ) ) ;
#5947 = CARTESIAN_POINT ( 'NONE',  ( 0.7868956173019259204, 9.000000000000000000, 7.903520140620750034 ) ) ;
#5948 = CARTESIAN_POINT ( 'NONE',  ( 1.650143266773734796, 0.000000000000000000, -14.90895795148410841 ) ) ;
#5949 = DIRECTION ( 'NONE',  ( -0.000000000000000000, -1.000000000000000000, -0.000000000000000000 ) ) ;
#5950 = FACE_OUTER_BOUND ( 'NONE', #2442, .T. ) ;
#5951 = CARTESIAN_POINT ( 'NONE',  ( 30.79786191028635400, 3.000000000000000000, -6.999232361977355765 ) ) ;
#5952 = CIRCLE ( 'NONE', #26, 0.1000000000000000472 ) ;
#5953 = PRESENTATION_LAYER_ASSIGNMENT (  '', '', ( #5288 ) ) ;
#5954 = ORIENTED_EDGE ( 'NONE', *, *, #4997, .T. ) ;
#5955 = ORIENTED_EDGE ( 'NONE', *, *, #11879, .T. ) ;
#5956 = EDGE_LOOP ( 'NONE', ( #12117, #9860, #4161, #10571 ) ) ;
#5957 = ORIENTED_EDGE ( 'NONE', *, *, #2184, .T. ) ;
#5958 = CARTESIAN_POINT ( 'NONE',  ( 8.252687871541629860, 3.000000000000000000, 31.00000000000000000 ) ) ;
#5959 = DIRECTION ( 'NONE',  ( -0.000000000000000000, -1.000000000000000000, -0.000000000000000000 ) ) ;
#5960 = AXIS2_PLACEMENT_3D ( 'NONE', #3080, #1155, #9285 ) ;
#5961 = VECTOR ( 'NONE', #139, 1000.000000000000000 ) ;
#5962 = LINE ( 'NONE', #3680, #7113 ) ;
#5963 = CARTESIAN_POINT ( 'NONE',  ( 30.80713437936438126, 0.000000000000000000, 0.9994049933487144655 ) ) ;
#5964 = CARTESIAN_POINT ( 'NONE',  ( 0.000000000000000000, 3.000000000000000000, 0.000000000000000000 ) ) ;
#5965 = EDGE_CURVE ( 'NONE', #9600, #10417, #5157, .T. ) ;
#5966 = CARTESIAN_POINT ( 'NONE',  ( 52.34174591811297717, 3.000000000000000000, -12.24483450274845531 ) ) ;
#5967 = CARTESIAN_POINT ( 'NONE',  ( 53.78299299645824050, 3.000000000000000000, -4.528231303176834643 ) ) ;
#5968 = ORIENTED_EDGE ( 'NONE', *, *, #8504, .F. ) ;
#5969 = CIRCLE ( 'NONE', #9700, 14.25000000000000178 ) ;
#5970 = EDGE_LOOP ( 'NONE', ( #11369, #10690, #2113, #1376 ) ) ;
#5971 = EDGE_LOOP ( 'NONE', ( #577, #11400, #6411, #7253 ) ) ;
#5972 = FACE_OUTER_BOUND ( 'NONE', #11296, .T. ) ;
#5973 = ORIENTED_EDGE ( 'NONE', *, *, #1701, .T. ) ;
#5974 = CARTESIAN_POINT ( 'NONE',  ( -2.161962830978785277, 3.000000000000000000, -14.08504230442586369 ) ) ;
#5975 = CLOSED_SHELL ( 'NONE', ( #4040, #2621, #13509, #2365, #2204, #11319, #5635, #8536, #1282, #10899, #2287, #1732, #1519, #10229, #5131, #12059, #614, #3809, #11496, #11703, #6756, #5292, #12938, #2695 ) ) ;
#5976 = DIRECTION ( 'NONE',  ( -0.6584756130119723272, -2.937361615894263844E-23, -0.7526020642202009281 ) ) ;
#5977 = VECTOR ( 'NONE', #7923, 1000.000000000000000 ) ;
#5978 = ADVANCED_FACE ( 'NONE', ( #4180 ), #10137, .T. ) ;
#5979 = FACE_OUTER_BOUND ( 'NONE', #2533, .T. ) ;
#5980 = DIRECTION ( 'NONE',  ( -0.000000000000000000, -1.000000000000000000, -0.000000000000000000 ) ) ;
#5981 = ADVANCED_FACE ( 'NONE', ( #11626 ), #6633, .F. ) ;
#5982 = DIRECTION ( 'NONE',  ( -0.000000000000000000, -1.000000000000000000, 0.000000000000000000 ) ) ;
#5983 = EDGE_CURVE ( 'NONE', #5440, #3458, #4630, .T. ) ;
#5984 = FACE_OUTER_BOUND ( 'NONE', #1648, .T. ) ;
#5985 = DIRECTION ( 'NONE',  ( -0.1453943818575021141, 0.000000000000000000, -0.9893737785712106714 ) ) ;
#5986 = ORIENTED_EDGE ( 'NONE', *, *, #9435, .F. ) ;
#5987 = DIRECTION ( 'NONE',  ( 0.000000000000000000, 0.000000000000000000, 1.000000000000000000 ) ) ;
#5988 = EDGE_CURVE ( 'NONE', #5397, #11577, #4118, .T. ) ;
#5989 = ORIENTED_EDGE ( 'NONE', *, *, #7018, .T. ) ;
#5990 = ORIENTED_EDGE ( 'NONE', *, *, #9541, .T. ) ;
#5991 = ORIENTED_EDGE ( 'NONE', *, *, #1049, .F. ) ;
#5992 = CARTESIAN_POINT ( 'NONE',  ( -2.631756770590896632, 3.000000000000000000, -14.20034848914872505 ) ) ;
#5993 = TOROIDAL_SURFACE ( 'NONE', #1821, 3.400000000000001243, 0.1000000000000000056 ) ;
#5994 = ORIENTED_EDGE ( 'NONE', *, *, #44, .F. ) ;
#5995 = CARTESIAN_POINT ( 'NONE',  ( -7.500000000000000000, 3.000000000000000000, 0.000000000000000000 ) ) ;
#5996 = VERTEX_POINT ( 'NONE', #6183 ) ;
#5997 = DIRECTION ( 'NONE',  ( -0.000000000000000000, -1.000000000000000000, -0.000000000000000000 ) ) ;
#5998 = SURFACE_STYLE_USAGE ( .BOTH. , #1877 ) ;
#5999 = CARTESIAN_POINT ( 'NONE',  ( -6.660869762029062890, 0.000000000000000000, -11.17001010193236610 ) ) ;
#6000 = ADVANCED_FACE ( 'NONE', ( #10389 ), #9362, .F. ) ;
#6001 = CYLINDRICAL_SURFACE ( 'NONE', #3294, 1.500000000000001332 ) ;
#6002 = AXIS2_PLACEMENT_3D ( 'NONE', #6277, #10342, #2085 ) ;
#6003 = DIRECTION ( 'NONE',  ( -0.000000000000000000, -1.000000000000000000, -0.000000000000000000 ) ) ;
#6004 = AXIS2_PLACEMENT_3D ( 'NONE', #10478, #11375, #5231 ) ;
#6005 = AXIS2_PLACEMENT_3D ( 'NONE', #13261, #13123, #7947 ) ;
#6006 = DIRECTION ( 'NONE',  ( -0.000000000000000000, -1.000000000000000000, 0.000000000000000000 ) ) ;
#6007 = DIRECTION ( 'NONE',  ( 0.000000000000000000, 1.000000000000000000, 0.000000000000000000 ) ) ;
#6008 = ORIENTED_EDGE ( 'NONE', *, *, #4482, .T. ) ;
#6009 = CARTESIAN_POINT ( 'NONE',  ( -5.733772933379472470, 3.000000000000000000, 13.04554897075799502 ) ) ;
#6010 = EDGE_CURVE ( 'NONE', #3195, #8124, #11010, .T. ) ;
#6011 = ORIENTED_EDGE ( 'NONE', *, *, #3006, .F. ) ;
#6012 = ORIENTED_EDGE ( 'NONE', *, *, #4556, .F. ) ;
#6013 = DIRECTION ( 'NONE',  ( 0.000000000000000000, 0.000000000000000000, -1.000000000000000000 ) ) ;
#6014 = EDGE_LOOP ( 'NONE', ( #5054, #12034, #9511, #4335 ) ) ;
#6015 = CIRCLE ( 'NONE', #4459, 0.1000000000000001166 ) ;
#6016 = AXIS2_PLACEMENT_3D ( 'NONE', #3813, #4917, #6025 ) ;
#6017 = AXIS2_PLACEMENT_3D ( 'NONE', #11380, #1945, #6138 ) ;
#6018 = CARTESIAN_POINT ( 'NONE',  ( 49.72134184781355515, 3.000000000000000000, -3.261665100124877981 ) ) ;
#6019 =( NAMED_UNIT ( * ) PLANE_ANGLE_UNIT ( ) SI_UNIT ( $, .RADIAN. ) );
#6020 = FACE_OUTER_BOUND ( 'NONE', #1909, .T. ) ;
#6021 = EDGE_CURVE ( 'NONE', #525, #4274, #1170, .T. ) ;
#6022 = CARTESIAN_POINT ( 'NONE',  ( -13.04554897075795949, 0.000000000000000000, 5.733772933379550629 ) ) ;
#6023 = EDGE_CURVE ( 'NONE', #3853, #5675, #4856, .T. ) ;
#6024 = CARTESIAN_POINT ( 'NONE',  ( -0.4399887592034530392, 9.000000000000000000, 8.488604708182295511 ) ) ;
#6025 = DIRECTION ( 'NONE',  ( 0.000000000000000000, 0.000000000000000000, 1.000000000000000000 ) ) ;
#6026 = CARTESIAN_POINT ( 'NONE',  ( -21.21140389626389577, 0.000000000000000000, -14.83930531255814955 ) ) ;
#6027 = CARTESIAN_POINT ( 'NONE',  ( 5.797378255456016483, 3.000000000000000000, 12.25282671965375592 ) ) ;
#6028 = AXIS2_PLACEMENT_3D ( 'NONE', #1758, #517, #7138 ) ;
#6029 = DIRECTION ( 'NONE',  ( 1.000000000000000000, 0.000000000000000000, 1.224646799147353207E-16 ) ) ;
#6030 = CYLINDRICAL_SURFACE ( 'NONE', #6005, 1.500000000000000222 ) ;
#6031 = AXIS2_PLACEMENT_3D ( 'NONE', #5433, #3289, #7505 ) ;
#6032 = ORIENTED_EDGE ( 'NONE', *, *, #8274, .T. ) ;
#6033 = B_SPLINE_CURVE_WITH_KNOTS ( 'NONE', 3,
 ( #7690, #397, #669, #605 ),
 .UNSPECIFIED., .F., .F.,
 ( 4, 4 ),
 ( 0.000000000000000000, 0.8452273900860258760 ),
 .UNSPECIFIED. ) ;
#6034 = ORIENTED_EDGE ( 'NONE', *, *, #2961, .F. ) ;
#6035 = EDGE_LOOP ( 'NONE', ( #9825, #4883, #5443, #4994 ) ) ;
#6036 = ORIENTED_EDGE ( 'NONE', *, *, #9169, .F. ) ;
#6037 = CARTESIAN_POINT ( 'NONE',  ( 2.720000000000001528, 2.000000000000000000, 4.500000000000000000 ) ) ;
#6038 = AXIS2_PLACEMENT_3D ( 'NONE', #10310, #814, #7152 ) ;
#6039 = VECTOR ( 'NONE', #9563, 1000.000000000000000 ) ;
#6040 = DIRECTION ( 'NONE',  ( 0.000000000000000000, 1.000000000000000000, 0.000000000000000000 ) ) ;
#6041 = EDGE_CURVE ( 'NONE', #12613, #11405, #6829, .T. ) ;
#6042 = EDGE_CURVE ( 'NONE', #357, #12112, #2148, .T. ) ;
#6043 = AXIS2_PLACEMENT_3D ( 'NONE', #1818, #9241, #1953 ) ;
#6044 = DIRECTION ( 'NONE',  ( -0.9248782281665488547, -0.000000000000000000, 0.3802634127332066294 ) ) ;
#6045 = DIRECTION ( 'NONE',  ( -0.000000000000000000, -1.000000000000000000, 0.000000000000000000 ) ) ;
#6046 = CARTESIAN_POINT ( 'NONE',  ( 0.000000000000000000, 0.000000000000000000, 0.000000000000000000 ) ) ;
#6047 = CARTESIAN_POINT ( 'NONE',  ( 31.00000000000000000, 2.900000000000000355, 0.000000000000000000 ) ) ;
#6048 = CIRCLE ( 'NONE', #8025, 14.25000000000000000 ) ;
#6049 = DIRECTION ( 'NONE',  ( 0.000000000000000000, 0.000000000000000000, 1.000000000000000000 ) ) ;
#6050 = VECTOR ( 'NONE', #12901, 1000.000000000000000 ) ;
#6051 = ORIENTED_EDGE ( 'NONE', *, *, #11459, .F. ) ;
#6052 = DIRECTION ( 'NONE',  ( 0.000000000000000000, 1.000000000000000000, -0.000000000000000000 ) ) ;
#6053 = DIRECTION ( 'NONE',  ( -0.000000000000000000, -1.000000000000000000, -0.000000000000000000 ) ) ;
#6054 = VERTEX_POINT ( 'NONE', #13067 ) ;
#6055 = CARTESIAN_POINT ( 'NONE',  ( -2.568302020731516588, 0.000000000000000000, -12.56087513340552242 ) ) ;
#6056 = B_SPLINE_CURVE_WITH_KNOTS ( 'NONE', 3,
 ( #13052, #5466, #5673, #248 ),
 .UNSPECIFIED., .F., .F.,
 ( 4, 4 ),
 ( 0.000000000000000000, 0.8724294488011784532 ),
 .UNSPECIFIED. ) ;
#6057 = CARTESIAN_POINT ( 'NONE',  ( 51.42634954137236036, 41.33135765298363395, -11.47886492887576182 ) ) ;
#6058 = DIRECTION ( 'NONE',  ( 0.000000000000000000, 1.000000000000000000, 0.000000000000000000 ) ) ;
#6059 = CARTESIAN_POINT ( 'NONE',  ( 7.065816209474156118, 3.000000000000000000, -10.69794375946289833 ) ) ;
#6060 = CARTESIAN_POINT ( 'NONE',  ( -11.11702303352191734, 3.000000000000000000, 8.914835885878279242 ) ) ;
#6061 = LINE ( 'NONE', #7092, #2035 ) ;
#6062 = CARTESIAN_POINT ( 'NONE',  ( -5.976238463952679325, 0.000000000000000000, -3.138004751744733589 ) ) ;
#6063 = ORIENTED_EDGE ( 'NONE', *, *, #1575, .T. ) ;
#6064 = FACE_OUTER_BOUND ( 'NONE', #771, .T. ) ;
#6065 = ORIENTED_EDGE ( 'NONE', *, *, #1969, .T. ) ;
#6066 = ORIENTED_EDGE ( 'NONE', *, *, #11561, .F. ) ;
#6067 = CARTESIAN_POINT ( 'NONE',  ( -2.830255545554292151, 3.000000000000000000, -12.68816982652971959 ) ) ;
#6068 = EDGE_CURVE ( 'NONE', #1235, #8499, #3457, .T. ) ;
#6069 = VERTEX_POINT ( 'NONE', #10787 ) ;
#6070 = CARTESIAN_POINT ( 'NONE',  ( -5.039625798601655937, 9.000000000000000000, 4.490509081392509927 ) ) ;
#6071 = CARTESIAN_POINT ( 'NONE',  ( 0.000000000000000000, 9.000000000000000000, 0.000000000000000000 ) ) ;
#6072 = DIRECTION ( 'NONE',  ( 0.000000000000000000, 0.000000000000000000, -1.000000000000000000 ) ) ;
#6073 = CARTESIAN_POINT ( 'NONE',  ( 7.065816209474156118, 3.000000000000000000, -10.69794375946289833 ) ) ;
#6074 = CARTESIAN_POINT ( 'NONE',  ( 1.133238802859644956, 3.000000000000000000, -14.39763212228013600 ) ) ;
#6075 = DIRECTION ( 'NONE',  ( -0.000000000000000000, -1.000000000000000000, -0.000000000000000000 ) ) ;
#6076 = CARTESIAN_POINT ( 'NONE',  ( -11.80615107470192804, 3.000000000000000000, -2.604399508764160487 ) ) ;
#6077 = EDGE_LOOP ( 'NONE', ( #502, #132 ) ) ;
#6078 = CARTESIAN_POINT ( 'NONE',  ( -13.28140389626389783, 3.000000000000000000, 13.39999999999999858 ) ) ;
#6079 = ORIENTED_EDGE ( 'NONE', *, *, #7812, .F. ) ;
#6080 = VERTEX_POINT ( 'NONE', #9754 ) ;
#6081 = DIRECTION ( 'NONE',  ( -2.312964634635743450E-15, -1.000000000000000000, 0.000000000000000000 ) ) ;
#6082 = EDGE_CURVE ( 'NONE', #1535, #6548, #456, .T. ) ;
#6083 = B_SPLINE_SURFACE_WITH_KNOTS ( 'NONE', 3, 1, ( 
 ( #8492, #4367 ),
 ( #1069, #2306 ),
 ( #9733, #12714 ),
 ( #4505, #2167 ) ),
 .UNSPECIFIED., .F., .F., .F.,
 ( 4, 4 ),
 ( 2, 2 ),
 ( 0.000000000000000000, 0.5855695330273008592 ),
 ( 0.000000000000000000, 1.000000000000000000 ),
 .UNSPECIFIED. ) ;
#6084 = EDGE_CURVE ( 'NONE', #7786, #597, #3547, .T. ) ;
#6085 = ORIENTED_EDGE ( 'NONE', *, *, #4305, .F. ) ;
#6086 =( REPRESENTATION_RELATIONSHIP ('NONE','NONE', #3798, #8461 ) REPRESENTATION_RELATIONSHIP_WITH_TRANSFORMATION ( #11185 )SHAPE_REPRESENTATION_RELATIONSHIP( ) );
#6087 = CARTESIAN_POINT ( 'NONE',  ( 13.50000000000000355, 3.000000000000000000, -8.550000000000000711 ) ) ;
#6088 = EDGE_CURVE ( 'NONE', #12927, #9922, #5478, .T. ) ;
#6089 = FACE_OUTER_BOUND ( 'NONE', #3884, .T. ) ;
#6090 = ADVANCED_FACE ( 'NONE', ( #4656 ), #12868, .F. ) ;
#6091 = CARTESIAN_POINT ( 'NONE',  ( 31.00000000000000000, 0.000000000000000000, 0.000000000000000000 ) ) ;
#6092 = DIRECTION ( 'NONE',  ( -0.000000000000000000, -1.000000000000000000, -0.000000000000000000 ) ) ;
#6093 = CARTESIAN_POINT ( 'NONE',  ( -5.170206418547117266, 3.000000000000000000, 13.27898586450088203 ) ) ;
#6094 = CARTESIAN_POINT ( 'NONE',  ( 5.280889752749253319, 0.000000000000000000, -6.660495733750448899 ) ) ;
#6095 = LINE ( 'NONE', #10230, #13206 ) ;
#6096 = CARTESIAN_POINT ( 'NONE',  ( -5.250000000000000000, 3.000000000000000000, -29.44078293894052933 ) ) ;
#6097 = DIRECTION ( 'NONE',  ( -0.000000000000000000, -1.000000000000000000, -0.000000000000000000 ) ) ;
#6098 = CARTESIAN_POINT ( 'NONE',  ( 10.72973591378220704, 0.000000000000000000, -5.571433138827823761 ) ) ;
#6099 = VERTEX_POINT ( 'NONE', #11830 ) ;
#6100 = ORIENTED_EDGE ( 'NONE', *, *, #3292, .F. ) ;
#6101 = EDGE_CURVE ( 'NONE', #8926, #8654, #394, .T. ) ;
#6102 = ORIENTED_EDGE ( 'NONE', *, *, #8436, .F. ) ;
#6103 = EDGE_LOOP ( 'NONE', ( #10673, #6744, #13545, #13000 ) ) ;
#6104 = CARTESIAN_POINT ( 'NONE',  ( -11.70905276178463872, 0.000000000000000000, -9.375397774054366806 ) ) ;
#6105 = CARTESIAN_POINT ( 'NONE',  ( -9.375397774054503586, 0.000000000000000000, -11.70905276178452503 ) ) ;
#6106 = DIRECTION ( 'NONE',  ( 0.000000000000000000, 1.000000000000000000, -0.000000000000000000 ) ) ;
#6107 = FACE_BOUND ( 'NONE', #6407, .T. ) ;
#6108 = FACE_OUTER_BOUND ( 'NONE', #5468, .T. ) ;
#6109 = CARTESIAN_POINT ( 'NONE',  ( -14.20034848914871795, 3.000000000000000000, 2.631756770590945482 ) ) ;
#6110 = CARTESIAN_POINT ( 'NONE',  ( 12.25282671965375592, 3.000000000000000000, -5.797378255456012930 ) ) ;
#6111 = ORIENTED_EDGE ( 'NONE', *, *, #1932, .T. ) ;
#6112 = B_SPLINE_SURFACE_WITH_KNOTS ( 'NONE', 3, 1, ( 
 ( #3166, #277 ),
 ( #11641, #4468 ),
 ( #4194, #5297 ),
 ( #7440, #2075 ) ),
 .UNSPECIFIED., .F., .F., .F.,
 ( 4, 4 ),
 ( 2, 2 ),
 ( 0.1547128134717859205, 1.000000000000000000 ),
 ( 0.000000000000000000, 1.000000000000000000 ),
 .UNSPECIFIED. ) ;
#6113 = EDGE_CURVE ( 'NONE', #5504, #3759, #2325, .T. ) ;
#6114 = LINE ( 'NONE', #10313, #11040 ) ;
#6115 = EDGE_CURVE ( 'NONE', #9457, #8335, #11462, .T. ) ;
#6116 = CARTESIAN_POINT ( 'NONE',  ( 50.46378962010818015, 3.000000000000000000, -4.178819016005276943 ) ) ;
#6117 = ORIENTED_EDGE ( 'NONE', *, *, #7932, .T. ) ;
#6118 = EDGE_CURVE ( 'NONE', #7648, #6374, #12574, .T. ) ;
#6119 = CARTESIAN_POINT ( 'NONE',  ( -9.573149624528719315, 0.000000000000000000, -8.795158114916407754 ) ) ;
#6120 = PRODUCT_CONTEXT ( 'NONE', #9850, 'mechanical' ) ;
#6121 = CARTESIAN_POINT ( 'NONE',  ( 0.5398653231797245766, 3.000000000000000000, -12.07794044664754018 ) ) ;
#6122 = DIRECTION ( 'NONE',  ( -0.000000000000000000, -1.000000000000000000, -0.000000000000000000 ) ) ;
#6123 = CARTESIAN_POINT ( 'NONE',  ( 5.733772933379453818, 0.000000000000000000, 13.04554897075800568 ) ) ;
#6124 = CARTESIAN_POINT ( 'NONE',  ( -12.68816982652953840, 3.000000000000000000, -2.830255545554093644 ) ) ;
#6125 = CARTESIAN_POINT ( 'NONE',  ( 6.736042615721505200, 9.000000000000000000, 5.184180733653466433 ) ) ;
#6126 = ORIENTED_EDGE ( 'NONE', *, *, #2285, .F. ) ;
#6127 = EDGE_LOOP ( 'NONE', ( #11793, #10931, #2572, #10191 ) ) ;
#6128 = LINE ( 'NONE', #9493, #7765 ) ;
#6129 = ORIENTED_EDGE ( 'NONE', *, *, #9444, .T. ) ;
#6130 = DIRECTION ( 'NONE',  ( 0.000000000000000000, 1.000000000000000000, 0.000000000000000000 ) ) ;
#6131 = CARTESIAN_POINT ( 'NONE',  ( 12.00000000000000888, 5.000000000000000888, -10.00000000000000000 ) ) ;
#6132 = CARTESIAN_POINT ( 'NONE',  ( 0.000000000000000000, 3.000000000000000000, 0.000000000000000000 ) ) ;
#6133 = B_SPLINE_CURVE_WITH_KNOTS ( 'NONE', 3,
 ( #7940, #1619, #2846, #12162 ),
 .UNSPECIFIED., .F., .F.,
 ( 4, 4 ),
 ( 0.3636321741318673806, 0.3930502511895355711 ),
 .UNSPECIFIED. ) ;
#6134 = CARTESIAN_POINT ( 'NONE',  ( 9.299128225235451239, 0.000000000000000000, -10.25006213149493561 ) ) ;
#6135 = CARTESIAN_POINT ( 'NONE',  ( -14.08504230442586369, 3.000000000000000000, 2.161962830978781724 ) ) ;
#6136 = EDGE_CURVE ( 'NONE', #1887, #7786, #684, .T. ) ;
#6137 = ORIENTED_EDGE ( 'NONE', *, *, #212, .T. ) ;
#6138 = DIRECTION ( 'NONE',  ( 0.000000000000000000, 0.000000000000000000, -1.000000000000000000 ) ) ;
#6139 = ORIENTED_EDGE ( 'NONE', *, *, #7532, .F. ) ;
#6140 = ORIENTED_EDGE ( 'NONE', *, *, #2217, .T. ) ;
#6141 = CARTESIAN_POINT ( 'NONE',  ( 2.458659560121116527, 9.000000000000000000, -8.136645080586040635 ) ) ;
#6142 = ORIENTED_EDGE ( 'NONE', *, *, #192, .T. ) ;
#6143 = LINE ( 'NONE', #9176, #8452 ) ;
#6144 = SURFACE_SIDE_STYLE ('',( #9321 ) ) ;
#6145 = CARTESIAN_POINT ( 'NONE',  ( -11.80612203322752585, 3.000000000000000000, 2.604531154829235362 ) ) ;
#6146 = DIRECTION ( 'NONE',  ( 0.000000000000000000, 1.000000000000000000, 0.000000000000000000 ) ) ;
#6147 = AXIS2_PLACEMENT_3D ( 'NONE', #11689, #2120, #6378 ) ;
#6148 = LINE ( 'NONE', #8215, #1995 ) ;
#6149 = CONTEXT_DEPENDENT_SHAPE_REPRESENTATION ( #9065, #195 ) ;
#6150 = CARTESIAN_POINT ( 'NONE',  ( 31.00000000000000000, 0.000000000000000000, -1.073670993220974656E-09 ) ) ;
#6151 = DIRECTION ( 'NONE',  ( -0.000000000000000000, -1.000000000000000000, -0.000000000000000000 ) ) ;
#6152 = CARTESIAN_POINT ( 'NONE',  ( -3.835481108877868195, 9.000000000000000000, 5.554420281491219136 ) ) ;
#6153 = DIRECTION ( 'NONE',  ( -3.469446951953610639E-15, -1.000000000000000000, 0.000000000000000000 ) ) ;
#6154 = EDGE_CURVE ( 'NONE', #2645, #8456, #13499, .T. ) ;
#6155 = ORIENTED_EDGE ( 'NONE', *, *, #8168, .T. ) ;
#6156 = CARTESIAN_POINT ( 'NONE',  ( 0.000000000000000000, 9.000000000000000000, 0.000000000000000000 ) ) ;
#6157 = ORIENTED_EDGE ( 'NONE', *, *, #4327, .F. ) ;
#6158 = EDGE_CURVE ( 'NONE', #12983, #3916, #10541, .T. ) ;
#6159 = ORIENTED_EDGE ( 'NONE', *, *, #6118, .T. ) ;
#6160 = EDGE_CURVE ( 'NONE', #4457, #6631, #5952, .T. ) ;
#6161 = AXIS2_PLACEMENT_3D ( 'NONE', #10725, #5945, #4710 ) ;
#6162 = ORIENTED_EDGE ( 'NONE', *, *, #2207, .F. ) ;
#6163 = ORIENTED_EDGE ( 'NONE', *, *, #12652, .F. ) ;
#6164 = CARTESIAN_POINT ( 'NONE',  ( 6.123233995736766282E-16, 3.000000000000000000, -5.000000000000000000 ) ) ;
#6165 = CARTESIAN_POINT ( 'NONE',  ( -9.299128225235689271, 0.000000000000000000, -10.25006213149501555 ) ) ;
#6166 = DIRECTION ( 'NONE',  ( 0.000000000000000000, 0.000000000000000000, -1.000000000000000000 ) ) ;
#6167 = CIRCLE ( 'NONE', #4184, 3.400000000000001243 ) ;
#6168 = EDGE_CURVE ( 'NONE', #11807, #4282, #12039, .T. ) ;
#6169 = DIRECTION ( 'NONE',  ( 0.000000000000000000, 0.000000000000000000, 1.000000000000000000 ) ) ;
#6170 = CARTESIAN_POINT ( 'NONE',  ( 45.60964950616533287, 3.000000000000000000, -14.50984893380129392 ) ) ;
#6171 =( GEOMETRIC_REPRESENTATION_CONTEXT ( 3 ) GLOBAL_UNCERTAINTY_ASSIGNED_CONTEXT ( ( #1586 ) ) GLOBAL_UNIT_ASSIGNED_CONTEXT ( ( #6895, #9992, #489 ) ) REPRESENTATION_CONTEXT ( 'NONE', 'WORKASPACE' ) );
#6172 = DIRECTION ( 'NONE',  ( 0.000000000000000000, 0.000000000000000000, 1.000000000000000000 ) ) ;
#6173 = LINE ( 'NONE', #3836, #6893 ) ;
#6174 = ORIENTED_EDGE ( 'NONE', *, *, #9373, .T. ) ;
#6175 = EDGE_CURVE ( 'NONE', #180, #4632, #12182, .T. ) ;
#6176 = CARTESIAN_POINT ( 'NONE',  ( 10.18979803820051622, 3.000000000000000000, -6.506620931068703761 ) ) ;
#6177 = CARTESIAN_POINT ( 'NONE',  ( 0.000000000000000000, 3.000000000000000000, 0.000000000000000000 ) ) ;
#6178 = AXIS2_PLACEMENT_3D ( 'NONE', #5772, #10803, #13084 ) ;
#6179 = VERTEX_POINT ( 'NONE', #1564 ) ;
#6180 = CARTESIAN_POINT ( 'NONE',  ( -4.577511697546077230, 3.000000000000000000, -12.75843939030334795 ) ) ;
#6181 = ADVANCED_FACE ( 'NONE', ( #11201 ), #7282, .F. ) ;
#6182 = CARTESIAN_POINT ( 'NONE',  ( -10.97318381393799136, 3.000000000000000000, -6.970598036433411693 ) ) ;
#6183 = CARTESIAN_POINT ( 'NONE',  ( 10.00000000000000888, 5.000000000000007994, -10.00000000000000000 ) ) ;
#6184 = EDGE_CURVE ( 'NONE', #3598, #7142, #6786, .T. ) ;
#6185 = AXIS2_PLACEMENT_3D ( 'NONE', #4230, #8425, #3202 ) ;
#6186 = DIRECTION ( 'NONE',  ( 0.000000000000000000, 0.000000000000000000, -1.000000000000000000 ) ) ;
#6187 = VECTOR ( 'NONE', #8497, 1000.000000000000000 ) ;
#6188 = AXIS2_PLACEMENT_3D ( 'NONE', #53, #4233, #9547 ) ;
#6189 = DIRECTION ( 'NONE',  ( 0.000000000000000000, 1.000000000000000000, 0.000000000000000000 ) ) ;
#6190 = CARTESIAN_POINT ( 'NONE',  ( -2.830255545554292151, 0.000000000000000000, -12.68816982652971959 ) ) ;
#6191 = ORIENTED_EDGE ( 'NONE', *, *, #3314, .T. ) ;
#6192 = ORIENTED_EDGE ( 'NONE', *, *, #6232, .F. ) ;
#6193 = DIRECTION ( 'NONE',  ( 0.6291930273683260522, 0.000000000000000000, -0.7772490812545749250 ) ) ;
#6194 = ORIENTED_EDGE ( 'NONE', *, *, #6175, .T. ) ;
#6195 = AXIS2_PLACEMENT_3D ( 'NONE', #7261, #12639, #10499 ) ;
#6196 = CARTESIAN_POINT ( 'NONE',  ( 2.392396671352951198, 0.000000000000000000, 6.311809420990095454 ) ) ;
#6197 = FILL_AREA_STYLE ('',( #4191 ) ) ;
#6198 = DIRECTION ( 'NONE',  ( 1.000000000000000000, -3.491481338843133355E-15, -2.602085213965210149E-16 ) ) ;
#6199 = CARTESIAN_POINT ( 'NONE',  ( -3.647599401157625376, 3.000000000000000000, -11.52662650599085836 ) ) ;
#6200 = EDGE_CURVE ( 'NONE', #6731, #523, #12018, .T. ) ;
#6201 = LINE ( 'NONE', #7380, #9976 ) ;
#6202 = CARTESIAN_POINT ( 'NONE',  ( -8.352599575481674421, 0.000000000000000000, 31.00000000000000000 ) ) ;
#6203 = LINE ( 'NONE', #6135, #12661 ) ;
#6204 = ORIENTED_EDGE ( 'NONE', *, *, #3752, .T. ) ;
#6205 = CIRCLE ( 'NONE', #3122, 8.500000000000000000 ) ;
#6206 = CARTESIAN_POINT ( 'NONE',  ( -11.52330688609014686, 3.000000000000000000, -6.017756925049552841 ) ) ;
#6207 = TOROIDAL_SURFACE ( 'NONE', #9720, 3.100000000000000533, 0.1000000000000000056 ) ;
#6208 = EDGE_LOOP ( 'NONE', ( #733, #9645, #2584, #10646 ) ) ;
#6209 = ORIENTED_EDGE ( 'NONE', *, *, #12925, .T. ) ;
#6210 = CARTESIAN_POINT ( 'NONE',  ( 1.836970198721030181E-16, 3.000000000000000000, 1.500000000000000222 ) ) ;
#6211 = ORIENTED_EDGE ( 'NONE', *, *, #1477, .T. ) ;
#6212 = EDGE_CURVE ( 'NONE', #9781, #5917, #6936, .T. ) ;
#6213 = DIRECTION ( 'NONE',  ( 0.000000000000000000, 1.000000000000000000, -0.000000000000000000 ) ) ;
#6214 = AXIS2_PLACEMENT_3D ( 'NONE', #6688, #1312, #5505 ) ;
#6215 = CARTESIAN_POINT ( 'NONE',  ( 8.795158114916441505, 3.000000000000000000, -9.573149624528689117 ) ) ;
#6216 = VECTOR ( 'NONE', #8142, 1000.000000000000000 ) ;
#6217 = VECTOR ( 'NONE', #12145, 1000.000000000000000 ) ;
#6218 = CARTESIAN_POINT ( 'NONE',  ( -5.571433138827826426, 0.000000000000000000, -10.72973591378220526 ) ) ;
#6219 = CARTESIAN_POINT ( 'NONE',  ( -12.68816982652970893, 3.000000000000000000, 2.830255545554337004 ) ) ;
#6220 = DIRECTION ( 'NONE',  ( 0.000000000000000000, 0.000000000000000000, 1.000000000000000000 ) ) ;
#6221 = CARTESIAN_POINT ( 'NONE',  ( 4.652003457867571967, 0.000000000000000000, -6.437678087145717321 ) ) ;
#6222 = CARTESIAN_POINT ( 'NONE',  ( 0.000000000000000000, 3.000000000000000000, 0.000000000000000000 ) ) ;
#6223 = DIRECTION ( 'NONE',  ( -0.000000000000000000, -1.000000000000000000, -0.000000000000000000 ) ) ;
#6224 = ORIENTED_EDGE ( 'NONE', *, *, #6021, .F. ) ;
#6225 = CARTESIAN_POINT ( 'NONE',  ( 0.000000000000000000, 3.000000000000000000, 0.000000000000000000 ) ) ;
#6226 = ORIENTED_EDGE ( 'NONE', *, *, #4321, .F. ) ;
#6227 = VECTOR ( 'NONE', #9145, 1000.000000000000000 ) ;
#6228 = ORIENTED_EDGE ( 'NONE', *, *, #1910, .F. ) ;
#6229 = CIRCLE ( 'NONE', #12611, 1.500000000000003997 ) ;
#6230 = AXIS2_PLACEMENT_3D ( 'NONE', #4138, #7384, #9171 ) ;
#6231 = ORIENTED_EDGE ( 'NONE', *, *, #321, .T. ) ;
#6232 = EDGE_CURVE ( 'NONE', #6390, #9536, #11520, .T. ) ;
#6233 = VERTEX_POINT ( 'NONE', #11137 ) ;
#6234 = CYLINDRICAL_SURFACE ( 'NONE', #5356, 1.499999999999997780 ) ;
#6235 = CARTESIAN_POINT ( 'NONE',  ( 9.250000000000003553, 2.750000000000000888, -10.00000000000000178 ) ) ;
#6236 = CARTESIAN_POINT ( 'NONE',  ( 10.14701493152832512, 3.000000000000000000, -29.73855628788322747 ) ) ;
#6237 = AXIS2_PLACEMENT_3D ( 'NONE', #10429, #3050, #5196 ) ;
#6238 = VECTOR ( 'NONE', #4800, 1000.000000000000000 ) ;
#6239 = DIRECTION ( 'NONE',  ( 0.000000000000000000, 0.000000000000000000, 1.000000000000000000 ) ) ;
#6240 = DIRECTION ( 'NONE',  ( 1.000000000000000000, -3.469446951953610639E-15, -2.602085213965210149E-16 ) ) ;
#6241 = ORIENTED_EDGE ( 'NONE', *, *, #13248, .F. ) ;
#6242 = CARTESIAN_POINT ( 'NONE',  ( -3.469446951953614189E-15, 2.000000000000000000, -6.999999999999998224 ) ) ;
#6243 = FACE_OUTER_BOUND ( 'NONE', #4520, .T. ) ;
#6244 = EDGE_CURVE ( 'NONE', #10564, #1235, #12991, .T. ) ;
#6245 = ORIENTED_EDGE ( 'NONE', *, *, #1115, .T. ) ;
#6246 = DIRECTION ( 'NONE',  ( 0.5610724890695777400, 0.000000000000000000, -0.8277666712360848278 ) ) ;
#6247 = DIRECTION ( 'NONE',  ( 0.000000000000000000, 0.000000000000000000, -1.000000000000000000 ) ) ;
#6248 = ADVANCED_FACE ( 'NONE', ( #4860 ), #5753, .F. ) ;
#6249 = APPLICATION_PROTOCOL_DEFINITION ( 'draft international standard', 'automotive_design', 1998, #8884 ) ;
#6250 = EDGE_CURVE ( 'NONE', #5694, #11681, #5925, .T. ) ;
#6251 = CARTESIAN_POINT ( 'NONE',  ( 8.883544964651964193, 0.000000000000000000, -12.08646469655236544 ) ) ;
#6252 = DIRECTION ( 'NONE',  ( 0.000000000000000000, 0.000000000000000000, -1.000000000000000000 ) ) ;
#6253 = CIRCLE ( 'NONE', #2092, 2.750000000000002665 ) ;
#6254 = CARTESIAN_POINT ( 'NONE',  ( -12.08646469655240097, 3.000000000000000000, -8.883544964651921561 ) ) ;
#6255 = AXIS2_PLACEMENT_3D ( 'NONE', #3417, #12870, #7629 ) ;
#6256 = DIRECTION ( 'NONE',  ( 0.000000000000000000, 1.000000000000000000, -0.000000000000000000 ) ) ;
#6257 = DIRECTION ( 'NONE',  ( 0.000000000000000000, -0.000000000000000000, 1.000000000000000000 ) ) ;
#6258 =( REPRESENTATION_RELATIONSHIP ('NONE','NONE', #3798, #7939 ) REPRESENTATION_RELATIONSHIP_WITH_TRANSFORMATION ( #5736 )SHAPE_REPRESENTATION_RELATIONSHIP( ) );
#6259 = ORIENTED_EDGE ( 'NONE', *, *, #8478, .F. ) ;
#6260 = ORIENTED_EDGE ( 'NONE', *, *, #2980, .F. ) ;
#6261 = DIRECTION ( 'NONE',  ( -0.000000000000000000, -1.000000000000000000, -0.000000000000000000 ) ) ;
#6262 = ADVANCED_FACE ( 'NONE', ( #4796 ), #13197, .T. ) ;
#6263 = VERTEX_POINT ( 'NONE', #3895 ) ;
#6264 = AXIS2_PLACEMENT_3D ( 'NONE', #2507, #2705, #507 ) ;
#6265 = AXIS2_PLACEMENT_3D ( 'NONE', #9995, #4697, #704 ) ;
#6266 = CARTESIAN_POINT ( 'NONE',  ( 0.000000000000000000, 0.000000000000000000, 0.000000000000000000 ) ) ;
#6267 = CARTESIAN_POINT ( 'NONE',  ( 6.553553527263006551, 9.000000000000000000, 1.616612558808879774 ) ) ;
#6268 = CARTESIAN_POINT ( 'NONE',  ( 0.000000000000000000, 9.000000000000000000, 0.000000000000000000 ) ) ;
#6269 = CARTESIAN_POINT ( 'NONE',  ( -9.375397774054503586, 0.000000000000000000, -11.70905276178452503 ) ) ;
#6270 = FACE_OUTER_BOUND ( 'NONE', #4432, .T. ) ;
#6271 = CARTESIAN_POINT ( 'NONE',  ( 50.46378962010818015, 3.000000000000000000, -4.178819016005276943 ) ) ;
#6272 = ORIENTED_EDGE ( 'NONE', *, *, #8085, .T. ) ;
#6273 = PRESENTATION_LAYER_ASSIGNMENT (  '', '', ( #11998 ) ) ;
#6274 = FACE_OUTER_BOUND ( 'NONE', #10583, .T. ) ;
#6275 = ORIENTED_EDGE ( 'NONE', *, *, #8265, .F. ) ;
#6276 = ORIENTED_EDGE ( 'NONE', *, *, #6505, .F. ) ;
#6277 = CARTESIAN_POINT ( 'NONE',  ( 41.29994854050690378, 0.000000000000000000, -5.141175130212632283 ) ) ;
#6278 = B_SPLINE_CURVE_WITH_KNOTS ( 'NONE', 3,
 ( #4162, #1972, #9589, #13475 ),
 .UNSPECIFIED., .F., .F.,
 ( 4, 4 ),
 ( 0.5454515525569062495, 0.5748696296145745510 ),
 .UNSPECIFIED. ) ;
#6279 = EDGE_CURVE ( 'NONE', #5890, #5239, #12675, .T. ) ;
#6280 = ORIENTED_EDGE ( 'NONE', *, *, #6088, .T. ) ;
#6281 = B_SPLINE_CURVE_WITH_KNOTS ( 'NONE', 2,
 ( #11104, #8807, #13104 ),
 .UNSPECIFIED., .F., .F.,
 ( 3, 3 ),
 ( 0.000000000000000000, 0.02941149433826504428 ),
 .UNSPECIFIED. ) ;
#6282 = CARTESIAN_POINT ( 'NONE',  ( -8.795158114916672432, 3.000000000000000000, -9.573149624528774382 ) ) ;
#6283 = AXIS2_PLACEMENT_3D ( 'NONE', #11287, #6951, #12267 ) ;
#6284 = FACE_OUTER_BOUND ( 'NONE', #12168, .T. ) ;
#6285 = CARTESIAN_POINT ( 'NONE',  ( -11.63517940784383775, 0.000000000000000000, -7.494008246337203083 ) ) ;
#6286 = DIRECTION ( 'NONE',  ( 0.000000000000000000, 0.000000000000000000, -1.000000000000000000 ) ) ;
#6287 = DIRECTION ( 'NONE',  ( 0.000000000000000000, 1.000000000000000000, 0.000000000000000000 ) ) ;
#6288 = FACE_OUTER_BOUND ( 'NONE', #8120, .T. ) ;
#6289 = DIRECTION ( 'NONE',  ( 0.000000000000000000, 0.000000000000000000, 1.000000000000000000 ) ) ;
#6290 = DIRECTION ( 'NONE',  ( 0.000000000000000000, 1.000000000000000000, 0.000000000000000000 ) ) ;
#6291 = ORIENTED_EDGE ( 'NONE', *, *, #3722, .T. ) ;
#6292 = CARTESIAN_POINT ( 'NONE',  ( -14.16466328168009881, 0.000000000000000000, 1.557181465540760534 ) ) ;
#6293 = ORIENTED_EDGE ( 'NONE', *, *, #3438, .F. ) ;
#6294 = ORIENTED_EDGE ( 'NONE', *, *, #8096, .F. ) ;
#6295 = ORIENTED_EDGE ( 'NONE', *, *, #8357, .F. ) ;
#6296 = ORIENTED_EDGE ( 'NONE', *, *, #857, .F. ) ;
#6297 = LINE ( 'NONE', #12314, #1634 ) ;
#6298 = CARTESIAN_POINT ( 'NONE',  ( 6.017756925049591921, 3.000000000000000000, -11.52330688609011844 ) ) ;
#6299 = DIRECTION ( 'NONE',  ( 0.000000000000000000, 0.000000000000000000, 1.000000000000000000 ) ) ;
#6300 = CARTESIAN_POINT ( 'NONE',  ( -11.48836750521723893, 0.000000000000000000, 8.430890348300625448 ) ) ;
#6301 = CARTESIAN_POINT ( 'NONE',  ( 0.000000000000000000, 13.00000000000000178, 0.000000000000000000 ) ) ;
#6302 = B_SPLINE_CURVE_WITH_KNOTS ( 'NONE', 3,
 ( #7059, #2785, #8148, #5818 ),
 .UNSPECIFIED., .F., .F.,
 ( 4, 4 ),
 ( 0.1547128134717859205, 1.000000000000000000 ),
 .UNSPECIFIED. ) ;
#6304 = CARTESIAN_POINT ( 'NONE',  ( -5.170206418547586225, 0.000000000000000000, 13.27898586450069907 ) ) ;
#6303 = B_SPLINE_CURVE_WITH_KNOTS ( 'NONE', 3,
 ( #9933, #11186, #5947, #1691 ),
 .UNSPECIFIED., .F., .F.,
 ( 4, 4 ),
 ( 0.000000000000000000, 0.8724294488011784532 ),
 .UNSPECIFIED. ) ;
#6305 = ORIENTED_EDGE ( 'NONE', *, *, #13327, .F. ) ;
#6306 = EDGE_CURVE ( 'NONE', #12681, #3357, #463, .T. ) ;
#6307 = ORIENTED_EDGE ( 'NONE', *, *, #4410, .T. ) ;
#6308 = FACE_OUTER_BOUND ( 'NONE', #4412, .T. ) ;
#6309 = DIRECTION ( 'NONE',  ( -0.000000000000000000, -1.000000000000000000, -0.000000000000000000 ) ) ;
#6310 = B_SPLINE_SURFACE_WITH_KNOTS ( 'NONE', 3, 1, ( 
 ( #6335, #6269 ),
 ( #1039, #12618 ),
 ( #4971, #13445 ),
 ( #3926, #12496 ) ),
 .UNSPECIFIED., .F., .F., .F.,
 ( 4, 4 ),
 ( 2, 2 ),
 ( 0.000000000000000000, 0.5855695330273008592 ),
 ( 0.000000000000000000, 1.000000000000000000 ),
 .UNSPECIFIED. ) ;
#6311 = VERTEX_POINT ( 'NONE', #3682 ) ;
#6312 = DIRECTION ( 'NONE',  ( 0.000000000000000000, 0.000000000000000000, 1.000000000000000000 ) ) ;
#6313 = LINE ( 'NONE', #10665, #1977 ) ;
#6314 = SHAPE_DEFINITION_REPRESENTATION ( #5429, #8461 ) ;
#6315 = CARTESIAN_POINT ( 'NONE',  ( 7.494008246337245716, 3.000000000000000000, -11.63517940784380578 ) ) ;
#6316 = CARTESIAN_POINT ( 'NONE',  ( 13.27898586450069907, 3.000000000000000000, 5.170206418547587113 ) ) ;
#6317 = DIRECTION ( 'NONE',  ( -0.000000000000000000, -1.000000000000000000, -0.000000000000000000 ) ) ;
#6318 = EDGE_CURVE ( 'NONE', #10298, #7353, #6410, .T. ) ;
#6319 = FACE_OUTER_BOUND ( 'NONE', #9674, .T. ) ;
#6320 = EDGE_CURVE ( 'NONE', #11737, #3918, #1344, .T. ) ;
#6321 = LINE ( 'NONE', #265, #8642 ) ;
#6322 = ORIENTED_EDGE ( 'NONE', *, *, #9888, .T. ) ;
#6323 = ORIENTED_EDGE ( 'NONE', *, *, #13471, .T. ) ;
#6324 = ADVANCED_FACE ( 'NONE', ( #4234 ), #2171, .F. ) ;
#6325 = ORIENTED_EDGE ( 'NONE', *, *, #10350, .T. ) ;
#6326 = LINE ( 'NONE', #11371, #7981 ) ;
#6327 = EDGE_CURVE ( 'NONE', #3598, #7043, #9871, .T. ) ;
#6328 = ORIENTED_EDGE ( 'NONE', *, *, #1453, .T. ) ;
#6329 = B_SPLINE_SURFACE_WITH_KNOTS ( 'NONE', 3, 1, ( 
 ( #800, #7134 ),
 ( #12378, #6991 ),
 ( #651, #13465 ),
 ( #1756, #12091 ) ),
 .UNSPECIFIED., .F., .F., .F.,
 ( 4, 4 ),
 ( 2, 2 ),
 ( 0.1547128134717859205, 1.000000000000000000 ),
 ( 0.000000000000000000, 1.000000000000000000 ),
 .UNSPECIFIED. ) ;
#6330 = CARTESIAN_POINT ( 'NONE',  ( -11.52666717836884125, 3.000000000000000000, -3.647470871583627705 ) ) ;
#6331 =( NAMED_UNIT ( * ) PLANE_ANGLE_UNIT ( ) SI_UNIT ( $, .RADIAN. ) );
#6332 = CARTESIAN_POINT ( 'NONE',  ( 3.647470871583629926, 0.000000000000000000, -11.52666717836884125 ) ) ;
#6333 = CARTESIAN_POINT ( 'NONE',  ( 30.73000000000000043, 3.000000000000000000, -3.999999999999999112 ) ) ;
#6334 = B_SPLINE_CURVE_WITH_KNOTS ( 'NONE', 3,
 ( #3237, #7511, #2348, #7709 ),
 .UNSPECIFIED., .F., .F.,
 ( 4, 4 ),
 ( 0.000000000000000000, 0.8724294488011776760 ),
 .UNSPECIFIED. ) ;
#6335 = CARTESIAN_POINT ( 'NONE',  ( -9.375397774054503586, 3.000000000000000000, -11.70905276178452503 ) ) ;
#6336 = PRODUCT_DEFINITION_SHAPE ( 'NONE', 'NONE',  #10940 ) ;
#6337 = ADVANCED_FACE ( 'NONE', ( #5337 ), #4166, .T. ) ;
#6338 = LINE ( 'NONE', #280, #471 ) ;
#6339 = CARTESIAN_POINT ( 'NONE',  ( 1.958311002203130480, 0.000000000000000000, -14.87484884897977366 ) ) ;
#6340 = VERTEX_POINT ( 'NONE', #1140 ) ;
#6341 = DIRECTION ( 'NONE',  ( 0.6291930273683203900, 0.000000000000000000, -0.7772490812545796990 ) ) ;
#6342 = ORIENTED_EDGE ( 'NONE', *, *, #5506, .T. ) ;
#6343 = ORIENTED_EDGE ( 'NONE', *, *, #5163, .T. ) ;
#6344 = ORIENTED_EDGE ( 'NONE', *, *, #3460, .F. ) ;
#6345 = CARTESIAN_POINT ( 'NONE',  ( -4.821006024661084410, 0.000000000000000000, -13.61374091949017640 ) ) ;
#6346 = ADVANCED_FACE ( 'NONE', ( #6108 ), #7151, .T. ) ;
#6347 = VERTEX_POINT ( 'NONE', #9410 ) ;
#6348 = DIRECTION ( 'NONE',  ( 0.000000000000000000, 1.000000000000000000, 0.000000000000000000 ) ) ;
#6349 = LINE ( 'NONE', #6415, #10461 ) ;
#6350 = CARTESIAN_POINT ( 'NONE',  ( 5.452638258930520010, 3.000000000000000000, -13.97385902380752754 ) ) ;
#6351 = CARTESIAN_POINT ( 'NONE',  ( -2.161962830978702677, 3.000000000000000000, 14.08504230442587435 ) ) ;
#6352 = CARTESIAN_POINT ( 'NONE',  ( -7.125870497355421662, 9.000000000000000000, -3.507536778237742237 ) ) ;
#6353 = EDGE_CURVE ( 'NONE', #8307, #3554, #4298, .T. ) ;
#6354 = CARTESIAN_POINT ( 'NONE',  ( -0.4399887592034473771, 0.000000000000000000, 8.488604708182295511 ) ) ;
#6355 = EDGE_CURVE ( 'NONE', #11639, #2029, #4426, .T. ) ;
#6356 = CARTESIAN_POINT ( 'NONE',  ( 6.736042615721505200, 0.000000000000000000, 5.184180733653466433 ) ) ;
#6357 = ORIENTED_EDGE ( 'NONE', *, *, #4597, .T. ) ;
#6358 = CARTESIAN_POINT ( 'NONE',  ( -8.922136023539609440, 3.000000000000000000, 8.158651161643900807 ) ) ;
#6359 = ORIENTED_EDGE ( 'NONE', *, *, #7784, .F. ) ;
#6360 = VERTEX_POINT ( 'NONE', #11477 ) ;
#6361 = B_SPLINE_CURVE_WITH_KNOTS ( 'NONE', 3,
 ( #1128, #9531, #8418, #4024 ),
 .UNSPECIFIED., .F., .F.,
 ( 4, 4 ),
 ( 0.1547128134717859205, 1.000000000000000000 ),
 .UNSPECIFIED. ) ;
#6362 = ORIENTED_EDGE ( 'NONE', *, *, #2194, .F. ) ;
#6363 = AXIS2_PLACEMENT_3D ( 'NONE', #13422, #883, #10178 ) ;
#6364 = CARTESIAN_POINT ( 'NONE',  ( 3.850308450823737516, 0.000000000000000000, 5.544152309732777617 ) ) ;
#6365 = FILL_AREA_STYLE ('',( #12584 ) ) ;
#6366 = CARTESIAN_POINT ( 'NONE',  ( 10.86210944460165528, 3.000000000000000000, 29.48017534571043541 ) ) ;
#6367 = FACE_OUTER_BOUND ( 'NONE', #3069, .T. ) ;
#6368 = CARTESIAN_POINT ( 'NONE',  ( -11.52330688609014686, 3.000000000000000000, -6.017756925049552841 ) ) ;
#6369 = CARTESIAN_POINT ( 'NONE',  ( 8.158551673544282679, 3.000000000000000000, -8.922226997226884393 ) ) ;
#6370 = CIRCLE ( 'NONE', #230, 14.25000000000000178 ) ;
#6371 = ORIENTED_EDGE ( 'NONE', *, *, #6763, .T. ) ;
#6372 = ORIENTED_EDGE ( 'NONE', *, *, #13578, .F. ) ;
#6373 = CARTESIAN_POINT ( 'NONE',  ( 9.600126836553261711, 0.000000000000000000, 8.482622935103766082 ) ) ;
#6374 = VERTEX_POINT ( 'NONE', #11349 ) ;
#6375 = CYLINDRICAL_SURFACE ( 'NONE', #3817, 1.500000000000000444 ) ;
#6376 = CIRCLE ( 'NONE', #13430, 1.000000000000001776 ) ;
#6377 = ADVANCED_FACE ( 'NONE', ( #7215 ), #1900, .F. ) ;
#6378 = DIRECTION ( 'NONE',  ( 0.000000000000000000, 0.000000000000000000, -1.000000000000000000 ) ) ;
#6379 = FACE_OUTER_BOUND ( 'NONE', #3420, .T. ) ;
#6380 = LINE ( 'NONE', #9484, #11675 ) ;
#6381 = CARTESIAN_POINT ( 'NONE',  ( 10.00000000000000533, 2.749999999999998224, 10.00000000000000000 ) ) ;
#6382 = FACE_OUTER_BOUND ( 'NONE', #13007, .T. ) ;
#6383 = FILL_AREA_STYLE_COLOUR ( '', #10422 ) ;
#6384 = VECTOR ( 'NONE', #5016, 1000.000000000000000 ) ;
#6385 = EDGE_LOOP ( 'NONE', ( #13374, #7635, #1711, #2178 ) ) ;
#6386=STYLED_ITEM('',(#13628),#3911);
#6387 = ORIENTED_EDGE ( 'NONE', *, *, #7418, .F. ) ;
#6388 = ORIENTED_EDGE ( 'NONE', *, *, #681, .T. ) ;
#6389 = DIRECTION ( 'NONE',  ( -0.3802634127332040759, -0.000000000000000000, -0.9248782281665499649 ) ) ;
#6390 = VERTEX_POINT ( 'NONE', #2043 ) ;
#6391 = EDGE_CURVE ( 'NONE', #11587, #5777, #4106, .T. ) ;
#6392 = ADVANCED_FACE ( 'NONE', ( #13550 ), #1918, .T. ) ;
#6393 = FACE_BOUND ( 'NONE', #7123, .T. ) ;
#6394 = EDGE_CURVE ( 'NONE', #4390, #11209, #50, .T. ) ;
#6395 = CIRCLE ( 'NONE', #5522, 6.750000000000000888 ) ;
#6396 = DIRECTION ( 'NONE',  ( 0.000000000000000000, 0.000000000000000000, -1.000000000000000000 ) ) ;
#6397 = AXIS2_PLACEMENT_3D ( 'NONE', #10318, #2877, #13361 ) ;
#6398 = DIRECTION ( 'NONE',  ( 0.000000000000000000, 0.000000000000000000, 1.000000000000000000 ) ) ;
#6399 = DIRECTION ( 'NONE',  ( -0.000000000000000000, -1.000000000000000000, -0.000000000000000000 ) ) ;
#6400 = EDGE_CURVE ( 'NONE', #6431, #11517, #8378, .T. ) ;
#6401 = CARTESIAN_POINT ( 'NONE',  ( 31.00000000000000000, 3.000000000000000000, 0.000000000000000000 ) ) ;
#6402 = FACE_OUTER_BOUND ( 'NONE', #786, .T. ) ;
#6403 = EDGE_LOOP ( 'NONE', ( #4295, #204, #10876, #12032 ) ) ;
#6404 = CARTESIAN_POINT ( 'NONE',  ( -13.50994833511691340, 3.000000000000000000, -1.105736515254444052 ) ) ;
#6405 = VERTEX_POINT ( 'NONE', #5268 ) ;
#6406 = VERTEX_POINT ( 'NONE', #9470 ) ;
#6407 = EDGE_LOOP ( 'NONE', ( #9414, #2628 ) ) ;
#6408 = CYLINDRICAL_SURFACE ( 'NONE', #2688, 12.08999999999737440 ) ;
#6409 = AXIS2_PLACEMENT_3D ( 'NONE', #1304, #5498, #9703 ) ;
#6411 = ORIENTED_EDGE ( 'NONE', *, *, #4762, .T. ) ;
#6410 = B_SPLINE_CURVE_WITH_KNOTS ( 'NONE', 3,
 ( #4733, #8920, #7883, #12105 ),
 .UNSPECIFIED., .F., .F.,
 ( 4, 4 ),
 ( 0.1276832474596270861, 1.000000000000000000 ),
 .UNSPECIFIED. ) ;
#6412 = B_SPLINE_SURFACE_WITH_KNOTS ( 'NONE', 3, 1, ( 
 ( #13255, #12089 ),
 ( #3667, #4916 ),
 ( #11121, #6773 ),
 ( #13334, #1689 ) ),
 .UNSPECIFIED., .F., .F., .F.,
 ( 4, 4 ),
 ( 2, 2 ),
 ( 0.1276832474596281686, 1.000000000000000000 ),
 ( 0.000000000000000000, 1.000000000000000000 ),
 .UNSPECIFIED. ) ;
#6413 = ADVANCED_FACE ( 'NONE', ( #11614 ), #13479, .F. ) ;
#6414 = DIRECTION ( 'NONE',  ( 0.000000000000000000, 0.000000000000000000, 1.000000000000000000 ) ) ;
#6415 = CARTESIAN_POINT ( 'NONE',  ( 2.719999999999997087, 2.000000000000000000, -4.500000000000000888 ) ) ;
#6416 = DIRECTION ( 'NONE',  ( 0.7772490812545874705, 0.000000000000000000, 0.6291930273683107311 ) ) ;
#6417 = LINE ( 'NONE', #4419, #9230 ) ;
#6418 = DIRECTION ( 'NONE',  ( -0.000000000000000000, -1.000000000000000000, -0.000000000000000000 ) ) ;
#6419 = AXIS2_PLACEMENT_3D ( 'NONE', #9273, #3967, #1981 ) ;
#6420 = EDGE_CURVE ( 'NONE', #5900, #3087, #5969, .T. ) ;
#6421 = CARTESIAN_POINT ( 'NONE',  ( 2.546103534247748712, 0.000000000000000000, -12.55526518755974585 ) ) ;
#6422 = EDGE_CURVE ( 'NONE', #12936, #2347, #3603, .T. ) ;
#6423 = VECTOR ( 'NONE', #1074, 1000.000000000000000 ) ;
#6424 = DIRECTION ( 'NONE',  ( 0.000000000000000000, 0.000000000000000000, -1.000000000000000000 ) ) ;
#6425 = CARTESIAN_POINT ( 'NONE',  ( 8.373678438139048552, 0.000000000000000000, 1.459968977288628178 ) ) ;
#6426 = ORIENTED_EDGE ( 'NONE', *, *, #4844, .T. ) ;
#6427 = CARTESIAN_POINT ( 'NONE',  ( 5.053288777954491273, 9.000000000000000000, -4.475128213425755952 ) ) ;
#6428 = B_SPLINE_SURFACE_WITH_KNOTS ( 'NONE', 3, 1, ( 
 ( #9656, #3514 ),
 ( #232, #8609 ),
 ( #12836, #5588 ),
 ( #10826, #2220 ) ),
 .UNSPECIFIED., .F., .F., .F.,
 ( 4, 4 ),
 ( 2, 2 ),
 ( 0.000000000000000000, 0.5855695330273008592 ),
 ( 0.000000000000000000, 1.000000000000000000 ),
 .UNSPECIFIED. ) ;
#6429 = ORIENTED_EDGE ( 'NONE', *, *, #4172, .T. ) ;
#6430 = VERTEX_POINT ( 'NONE', #5672 ) ;
#6431 = VERTEX_POINT ( 'NONE', #10915 ) ;
#6432 = AXIS2_PLACEMENT_3D ( 'NONE', #10136, #12149, #6013 ) ;
#6433 = CIRCLE ( 'NONE', #8833, 8.499999999999998224 ) ;
#6434 = CIRCLE ( 'NONE', #11717, 1.000000000000000888 ) ;
#6435 = EDGE_CURVE ( 'NONE', #97, #1924, #4311, .T. ) ;
#6436 = CARTESIAN_POINT ( 'NONE',  ( -6.515098946627274401, 9.000000000000000000, 3.430563300314522390 ) ) ;
#6437 = DIRECTION ( 'NONE',  ( -0.5366322685380731095, 0.000000000000000000, -0.8438162171727212613 ) ) ;
#6438 = CARTESIAN_POINT ( 'NONE',  ( -10.67828022838850721, 0.000000000000000000, 7.077546079049267469 ) ) ;
#6439 = CARTESIAN_POINT ( 'NONE',  ( 1.836970198721030181E-16, 3.000000000000000000, 1.500000000000000222 ) ) ;
#6440 = AXIS2_PLACEMENT_3D ( 'NONE', #11433, #6130, #8263 ) ;
#6441 = B_SPLINE_CURVE_WITH_KNOTS ( 'NONE', 3,
 ( #4211, #6739, #3187, #6492 ),
 .UNSPECIFIED., .F., .F.,
 ( 4, 4 ),
 ( 0.000000000000000000, 0.8724294488011762327 ),
 .UNSPECIFIED. ) ;
#6442 = CIRCLE ( 'NONE', #7332, 8.500000000000000000 ) ;
#6443 = CARTESIAN_POINT ( 'NONE',  ( -13.49999999999999645, 3.000000000000000000, -5.549999999999999822 ) ) ;
#6444 = AXIS2_PLACEMENT_3D ( 'NONE', #6071, #11892, #454 ) ;
#6445 = PRESENTATION_LAYER_ASSIGNMENT (  '', '', ( #11512 ) ) ;
#6446 = EDGE_LOOP ( 'NONE', ( #9569, #8187, #10621, #542 ) ) ;
#6447 = ORIENTED_EDGE ( 'NONE', *, *, #1041, .T. ) ;
#6448 = CARTESIAN_POINT ( 'NONE',  ( 11.11702303352196708, 3.000000000000000000, 8.914835885878218846 ) ) ;
#6449 = EDGE_CURVE ( 'NONE', #12461, #2370, #7294, .T. ) ;
#6450 = EDGE_CURVE ( 'NONE', #3357, #9908, #12717, .T. ) ;
#6451 = ORIENTED_EDGE ( 'NONE', *, *, #7406, .T. ) ;
#6452 = DIRECTION ( 'NONE',  ( 0.000000000000000000, 0.000000000000000000, -1.000000000000000000 ) ) ;
#6453 = CIRCLE ( 'NONE', #516, 1.499999999999997780 ) ;
#6454 = PRODUCT_DEFINITION_SHAPE ( 'NONE', 'NONE',  #13616 ) ;
#6455 = CIRCLE ( 'NONE', #11955, 1.500000000000000222 ) ;
#6456 = CARTESIAN_POINT ( 'NONE',  ( 10.97318381393774089, 3.000000000000000000, -6.970598036433387712 ) ) ;
#6457 = CARTESIAN_POINT ( 'NONE',  ( -4.227250083625790467, 0.000000000000000000, -13.17831234185026013 ) ) ;
#6458 = DIRECTION ( 'NONE',  ( 0.000000000000000000, 1.000000000000000000, -0.000000000000000000 ) ) ;
#6459 = CARTESIAN_POINT ( 'NONE',  ( -8.760376775873710997, 0.000000000000000000, 10.34346111134700941 ) ) ;
#6460 = DIRECTION ( 'NONE',  ( -0.000000000000000000, -1.000000000000000000, -0.000000000000000000 ) ) ;
#6461 = AXIS2_PLACEMENT_3D ( 'NONE', #13347, #4932, #7274 ) ;
#6462 = CARTESIAN_POINT ( 'NONE',  ( 28.54655175640005282, 0.000000000000000000, -2.353846153846155254 ) ) ;
#6463 = CIRCLE ( 'NONE', #7564, 12.08999999999737440 ) ;
#6464 = ORIENTED_EDGE ( 'NONE', *, *, #6518, .T. ) ;
#6465 = ORIENTED_EDGE ( 'NONE', *, *, #6570, .T. ) ;
#6466 = ORIENTED_EDGE ( 'NONE', *, *, #2619, .T. ) ;
#6467 = CARTESIAN_POINT ( 'NONE',  ( 8.914835885878220623, 3.000000000000000000, -11.11702303352196708 ) ) ;
#6468 = ORIENTED_EDGE ( 'NONE', *, *, #4889, .T. ) ;
#6469 = DIRECTION ( 'NONE',  ( 0.000000000000000000, 1.000000000000000000, -0.000000000000000000 ) ) ;
#6470 = AXIS2_PLACEMENT_3D ( 'NONE', #3552, #6940, #13069 ) ;
#6471 = SURFACE_STYLE_FILL_AREA ( #6197 ) ;
#6472 = TOROIDAL_SURFACE ( 'NONE', #541, 1.600000000000000311, 0.1000000000000000056 ) ;
#6473 = CARTESIAN_POINT ( 'NONE',  ( 4.821006024660968947, 0.000000000000000000, -13.61374091949021015 ) ) ;
#6474 = DIRECTION ( 'NONE',  ( 0.000000000000000000, 0.000000000000000000, 1.000000000000000000 ) ) ;
#6475 = CARTESIAN_POINT ( 'NONE',  ( -2.264806262022998062, 3.000000000000000000, -14.82803603298499340 ) ) ;
#6476 = CARTESIAN_POINT ( 'NONE',  ( -6.057461899949976747, 9.000000000000000000, 5.137313564148215939 ) ) ;
#6477 = CARTESIAN_POINT ( 'NONE',  ( -13.97385902380755240, 0.000000000000000000, -5.452638258930474713 ) ) ;
#6478 = EDGE_LOOP ( 'NONE', ( #6291, #6579, #9389, #2802 ) ) ;
#6479 = CYLINDRICAL_SURFACE ( 'NONE', #4248, 14.25000000000000178 ) ;
#6480 = ORIENTED_EDGE ( 'NONE', *, *, #264, .F. ) ;
#6481 = VERTEX_POINT ( 'NONE', #9737 ) ;
#6482 = EDGE_CURVE ( 'NONE', #2068, #11685, #10366, .T. ) ;
#6483 = CIRCLE ( 'NONE', #772, 12.99999999999977973 ) ;
#6484 = VERTEX_POINT ( 'NONE', #3260 ) ;
#6485 = VECTOR ( 'NONE', #3052, 1000.000000000000000 ) ;
#6486 = LINE ( 'NONE', #1250, #12169 ) ;
#6487 = ORIENTED_EDGE ( 'NONE', *, *, #7078, .T. ) ;
#6488 = DIRECTION ( 'NONE',  ( 0.000000000000000000, 0.000000000000000000, 1.000000000000000000 ) ) ;
#6489 = DIRECTION ( 'NONE',  ( -0.000000000000000000, -1.000000000000000000, -0.000000000000000000 ) ) ;
#6490 = DIRECTION ( 'NONE',  ( 0.000000000000000000, 0.000000000000000000, -1.000000000000000000 ) ) ;
#6491 = CARTESIAN_POINT ( 'NONE',  ( -8.883544964652065445, 0.000000000000000000, -12.08646469655229438 ) ) ;
#6492 = CARTESIAN_POINT ( 'NONE',  ( -2.481593227817850966, 0.000000000000000000, -8.129679886173169834 ) ) ;
#6493 =( GEOMETRIC_REPRESENTATION_CONTEXT ( 3 ) GLOBAL_UNCERTAINTY_ASSIGNED_CONTEXT ( ( #896 ) ) GLOBAL_UNIT_ASSIGNED_CONTEXT ( ( #12069, #13102, #2561 ) ) REPRESENTATION_CONTEXT ( 'NONE', 'WORKASPACE' ) );
#6494 = CARTESIAN_POINT ( 'NONE',  ( 8.914835885878215294, 3.000000000000000000, 11.11702303352197418 ) ) ;
#6495 = AXIS2_PLACEMENT_3D ( 'NONE', #13566, #2061, #11897 ) ;
#6496 = LINE ( 'NONE', #8071, #5529 ) ;
#6497 = CARTESIAN_POINT ( 'NONE',  ( -5.250000000000000000, 0.000000000000000000, -27.94078293894052578 ) ) ;
#6498 = VERTEX_POINT ( 'NONE', #382 ) ;
#6499 = CARTESIAN_POINT ( 'NONE',  ( 3.893011711613070691, 3.000000000000000000, -12.40340517008307231 ) ) ;
#6500 = ADVANCED_FACE ( 'NONE', ( #8702 ), #11021, .T. ) ;
#6501 = EDGE_LOOP ( 'NONE', ( #4239, #9424, #7478, #3519 ) ) ;
#6502 = EDGE_CURVE ( 'NONE', #8926, #9781, #9912, .T. ) ;
#6503 = ORIENTED_EDGE ( 'NONE', *, *, #2669, .T. ) ;
#6504 = ORIENTED_EDGE ( 'NONE', *, *, #1773, .F. ) ;
#6505 = EDGE_CURVE ( 'NONE', #7204, #7585, #1802, .T. ) ;
#6506 = ADVANCED_FACE ( 'NONE', ( #11677 ), #11419, .F. ) ;
#6507 = CARTESIAN_POINT ( 'NONE',  ( 12.57851281883977457, 3.000000000000000000, 3.283445639306028063 ) ) ;
#6508 = CARTESIAN_POINT ( 'NONE',  ( 2.394769219159762930, 1.734723475976807094E-15, -6.310909632292713844 ) ) ;
#6509 = CARTESIAN_POINT ( 'NONE',  ( 3.647470871583629926, 3.000000000000000000, -11.52666717836884125 ) ) ;
#6510 = CARTESIAN_POINT ( 'NONE',  ( -1.958311002203252160, 3.000000000000000000, -14.87484884897975768 ) ) ;
#6511 = CARTESIAN_POINT ( 'NONE',  ( 26.30958424017656938, 0.09999999999999982514, 4.500000000000000888 ) ) ;
#6512 = AXIS2_PLACEMENT_3D ( 'NONE', #5082, #3017, #3401 ) ;
#6513 = DIRECTION ( 'NONE',  ( 0.000000000000000000, 1.000000000000000000, 0.000000000000000000 ) ) ;
#6514 = EDGE_CURVE ( 'NONE', #13346, #9675, #10773, .T. ) ;
#6515 = ORIENTED_EDGE ( 'NONE', *, *, #13551, .T. ) ;
#6516 = ORIENTED_EDGE ( 'NONE', *, *, #12652, .T. ) ;
#6517 = DIRECTION ( 'NONE',  ( 0.000000000000000000, 0.000000000000000000, -1.000000000000000000 ) ) ;
#6518 = EDGE_CURVE ( 'NONE', #313, #9964, #10, .T. ) ;
#6519 = VERTEX_POINT ( 'NONE', #4438 ) ;
#6520 = CARTESIAN_POINT ( 'NONE',  ( 0.000000000000000000, 0.000000000000000000, 0.000000000000000000 ) ) ;
#6521 =( REPRESENTATION_RELATIONSHIP ('NONE','NONE', #3798, #8539 ) REPRESENTATION_RELATIONSHIP_WITH_TRANSFORMATION ( #588 )SHAPE_REPRESENTATION_RELATIONSHIP( ) );
#6522 = DIRECTION ( 'NONE',  ( 0.000000000000000000, 0.000000000000000000, 1.000000000000000000 ) ) ;
#6523 = CARTESIAN_POINT ( 'NONE',  ( -4.821006024661084410, 0.000000000000000000, -13.61374091949017640 ) ) ;
#6524 = CARTESIAN_POINT ( 'NONE',  ( -13.27898586450070084, 0.000000000000000000, -5.170206418547588001 ) ) ;
#6525 = DIRECTION ( 'NONE',  ( -0.000000000000000000, -1.000000000000000000, -0.000000000000000000 ) ) ;
#6526 = EDGE_CURVE ( 'NONE', #11178, #2755, #3404, .T. ) ;
#6527 = CARTESIAN_POINT ( 'NONE',  ( 6.025412986832064277, 0.000000000000000000, -13.73660796332615597 ) ) ;
#6528 = EDGE_CURVE ( 'NONE', #4567, #12679, #10847, .T. ) ;
#6529 = CARTESIAN_POINT ( 'NONE',  ( 1.557181465540672161, 0.000000000000000000, -14.16466328168010591 ) ) ;
#6530 = ORIENTED_EDGE ( 'NONE', *, *, #4572, .F. ) ;
#6531 = EDGE_LOOP ( 'NONE', ( #7567, #8424, #5079, #2909 ) ) ;
#6532 = ORIENTED_EDGE ( 'NONE', *, *, #8436, .T. ) ;
#6533 = ORIENTED_EDGE ( 'NONE', *, *, #888, .T. ) ;
#6534 = DIRECTION ( 'NONE',  ( 0.000000000000000000, 1.000000000000000000, -0.000000000000000000 ) ) ;
#6535 = ORIENTED_EDGE ( 'NONE', *, *, #11243, .F. ) ;
#6536 = DIRECTION ( 'NONE',  ( 0.000000000000000000, -0.000000000000000000, -1.000000000000000000 ) ) ;
#6538 = B_SPLINE_CURVE_WITH_KNOTS ( 'NONE', 3,
 ( #9834, #6677, #10880, #4604 ),
 .UNSPECIFIED., .F., .F.,
 ( 4, 4 ),
 ( 0.1547128134717859205, 1.000000000000000000 ),
 .UNSPECIFIED. ) ;
#6537 = SHAPE_REPRESENTATION ( 'base-mounting-bracket', ( #10007 ), #12660 ) ;
#6539 =( NAMED_UNIT ( * ) PLANE_ANGLE_UNIT ( ) SI_UNIT ( $, .RADIAN. ) );
#6540 = B_SPLINE_SURFACE_WITH_KNOTS ( 'NONE', 3, 1, ( 
 ( #3748, #7750 ),
 ( #7953, #8712 ),
 ( #12929, #2726 ),
 ( #11966, #1427 ) ),
 .UNSPECIFIED., .F., .F., .F.,
 ( 4, 4 ),
 ( 2, 2 ),
 ( 0.1547128134717859205, 1.000000000000000000 ),
 ( 0.000000000000000000, 1.000000000000000000 ),
 .UNSPECIFIED. ) ;
#6541 = CARTESIAN_POINT ( 'NONE',  ( 4.056222772158357692, 3.000000000000000000, -12.16218796965919680 ) ) ;
#6542 = DIRECTION ( 'NONE',  ( 0.000000000000000000, 1.000000000000000000, 0.000000000000000000 ) ) ;
#6543 = FACE_OUTER_BOUND ( 'NONE', #622, .T. ) ;
#6544 = DIRECTION ( 'NONE',  ( 0.000000000000000000, 1.000000000000000000, -0.000000000000000000 ) ) ;
#6545 = CARTESIAN_POINT ( 'NONE',  ( 10.97318381393774089, 0.000000000000000000, -6.970598036433387712 ) ) ;
#6546 = ORIENTED_EDGE ( 'NONE', *, *, #11908, .F. ) ;
#6547 =( NAMED_UNIT ( * ) PLANE_ANGLE_UNIT ( ) SI_UNIT ( $, .RADIAN. ) );
#6548 = VERTEX_POINT ( 'NONE', #5609 ) ;
#6549 = ORIENTED_EDGE ( 'NONE', *, *, #6526, .T. ) ;
#6550 = ORIENTED_EDGE ( 'NONE', *, *, #4799, .F. ) ;
#6551 = DIRECTION ( 'NONE',  ( 0.000000000000000000, 0.000000000000000000, 1.000000000000000000 ) ) ;
#6552 = ORIENTED_EDGE ( 'NONE', *, *, #12415, .T. ) ;
#6553 = ORIENTED_EDGE ( 'NONE', *, *, #9313, .T. ) ;
#6554 = DIRECTION ( 'NONE',  ( 0.000000000000000000, 0.000000000000000000, -1.000000000000000000 ) ) ;
#6555 =( NAMED_UNIT ( * ) SI_UNIT ( $, .STERADIAN. ) SOLID_ANGLE_UNIT ( ) );
#6556 = FACE_OUTER_BOUND ( 'NONE', #10155, .T. ) ;
#6557 = CARTESIAN_POINT ( 'NONE',  ( 0.000000000000000000, 0.000000000000000000, 0.000000000000000000 ) ) ;
#6558 = EDGE_CURVE ( 'NONE', #523, #7235, #7070, .T. ) ;
#6559 = CARTESIAN_POINT ( 'NONE',  ( 51.38094353598858532, 0.000000000000000000, -3.436371243710653722 ) ) ;
#6560 = LINE ( 'NONE', #5390, #924 ) ;
#6561 = LINE ( 'NONE', #8547, #11556 ) ;
#6562 = ORIENTED_EDGE ( 'NONE', *, *, #2447, .T. ) ;
#6563 = CARTESIAN_POINT ( 'NONE',  ( 29.02231267299996986, 3.000000000000000000, -1.321950885510182250 ) ) ;
#6564 = ORIENTED_EDGE ( 'NONE', *, *, #11661, .F. ) ;
#6565 = EDGE_LOOP ( 'NONE', ( #5954, #6012, #6751, #1797 ) ) ;
#6566 = ORIENTED_EDGE ( 'NONE', *, *, #10540, .T. ) ;
#6567 = CARTESIAN_POINT ( 'NONE',  ( 7.758214145541979967, 0.000000000000000000, 1.700281702449083054 ) ) ;
#6568 = CARTESIAN_POINT ( 'NONE',  ( 0.000000000000000000, 3.000000000000000000, 0.000000000000000000 ) ) ;
#6569 = ADVANCED_FACE ( 'NONE', ( #3533 ), #6843, .T. ) ;
#6570 = EDGE_CURVE ( 'NONE', #6347, #11521, #12585, .T. ) ;
#6571 = CARTESIAN_POINT ( 'NONE',  ( -7.751044794789887504, 9.000000000000000000, 1.733822342365972879 ) ) ;
#6572 = CYLINDRICAL_SURFACE ( 'NONE', #10334, 2.000000000000000444 ) ;
#6573 = DIRECTION ( 'NONE',  ( 0.000000000000000000, 0.000000000000000000, 1.000000000000000000 ) ) ;
#6574 = CARTESIAN_POINT ( 'NONE',  ( 2.830255545554135832, 3.000000000000000000, -12.68816982652952596 ) ) ;
#6575 = EDGE_CURVE ( 'NONE', #10694, #11321, #9042, .T. ) ;
#6576 = ORIENTED_EDGE ( 'NONE', *, *, #12994, .F. ) ;
#6577 = ORIENTED_EDGE ( 'NONE', *, *, #3335, .F. ) ;
#6578 = DIRECTION ( 'NONE',  ( -0.000000000000000000, -1.000000000000000000, -0.000000000000000000 ) ) ;
#6579 = ORIENTED_EDGE ( 'NONE', *, *, #5222, .F. ) ;
#6580 = CARTESIAN_POINT ( 'NONE',  ( -12.40347894490204794, 3.000000000000000000, 3.892776652129663173 ) ) ;
#6581 = EDGE_CURVE ( 'NONE', #12363, #7170, #3881, .T. ) ;
#6582 = CARTESIAN_POINT ( 'NONE',  ( -11.46814821560793440, 3.000000000000000000, 5.731782959214994477 ) ) ;
#6583 = CARTESIAN_POINT ( 'NONE',  ( -13.04554897075799680, 3.000000000000000000, -5.733772933379471581 ) ) ;
#6584 = DIRECTION ( 'NONE',  ( 0.000000000000000000, -0.000000000000000000, -1.000000000000000000 ) ) ;
#6585 = DIRECTION ( 'NONE',  ( 0.000000000000000000, 0.000000000000000000, 1.000000000000000000 ) ) ;
#6586 = CIRCLE ( 'NONE', #5695, 0.09999999999999982514 ) ;
#6587 = CARTESIAN_POINT ( 'NONE',  ( 2.453448243599948952, 0.1000000000000000056, 2.353846153846153921 ) ) ;
#6588 = EDGE_CURVE ( 'NONE', #2370, #12461, #7500, .T. ) ;
#6589 = DIRECTION ( 'NONE',  ( -0.000000000000000000, -1.000000000000000000, -0.000000000000000000 ) ) ;
#6590 = CARTESIAN_POINT ( 'NONE',  ( 3.647599401157691101, 0.000000000000000000, 11.52662650599084238 ) ) ;
#6591 = VERTEX_POINT ( 'NONE', #1757 ) ;
#6592 = ORIENTED_EDGE ( 'NONE', *, *, #181, .F. ) ;
#6593 = ORIENTED_EDGE ( 'NONE', *, *, #9312, .F. ) ;
#6594 = ORIENTED_EDGE ( 'NONE', *, *, #10199, .T. ) ;
#6595 = CARTESIAN_POINT ( 'NONE',  ( 0.000000000000000000, 3.000000000000000000, -1.500000000000000222 ) ) ;
#6596 = CIRCLE ( 'NONE', #4394, 3.400000000000001243 ) ;
#6597 = CIRCLE ( 'NONE', #1539, 12.08999999999737440 ) ;
#6598 = ORIENTED_EDGE ( 'NONE', *, *, #5828, .F. ) ;
#6599 = EDGE_CURVE ( 'NONE', #3596, #12785, #4784, .T. ) ;
#6600 = EDGE_CURVE ( 'NONE', #8692, #12875, #8972, .T. ) ;
#6601 = FACE_OUTER_BOUND ( 'NONE', #8316, .T. ) ;
#6602 = FACE_OUTER_BOUND ( 'NONE', #5956, .T. ) ;
#6603 = CARTESIAN_POINT ( 'NONE',  ( 20.00000000000000355, 3.000000000000000000, -14.92471123914604370 ) ) ;
#6604 = EDGE_CURVE ( 'NONE', #11919, #1456, #13337, .T. ) ;
#6605 = AXIS2_PLACEMENT_3D ( 'NONE', #8904, #1618, #13047 ) ;
#6606 = CARTESIAN_POINT ( 'NONE',  ( 8.883544964651964193, 0.000000000000000000, -12.08646469655236544 ) ) ;
#6607 = B_SPLINE_SURFACE_WITH_KNOTS ( 'NONE', 3, 1, ( 
 ( #8636, #11822 ),
 ( #10778, #6373 ),
 ( #3336, #8437 ),
 ( #10659, #7620 ) ),
 .UNSPECIFIED., .F., .F., .F.,
 ( 4, 4 ),
 ( 2, 2 ),
 ( 0.1547128134717859205, 1.000000000000000000 ),
 ( 0.000000000000000000, 1.000000000000000000 ),
 .UNSPECIFIED. ) ;
#6608 = AXIS2_PLACEMENT_3D ( 'NONE', #6268, #2263, #5233 ) ;
#6609 = CYLINDRICAL_SURFACE ( 'NONE', #10008, 12.08999999999737440 ) ;
#6610 = ORIENTED_EDGE ( 'NONE', *, *, #4510, .F. ) ;
#6611 = CARTESIAN_POINT ( 'NONE',  ( 8.481367827640703183, 9.000000000000000000, 0.5624942419805127880 ) ) ;
#6612 = ORIENTED_EDGE ( 'NONE', *, *, #9366, .T. ) ;
#6613 = EDGE_LOOP ( 'NONE', ( #6863, #12711, #11373, #9162 ) ) ;
#6614 = ORIENTED_EDGE ( 'NONE', *, *, #737, .T. ) ;
#6615 = LINE ( 'NONE', #13095, #942 ) ;
#6616 = VERTEX_POINT ( 'NONE', #8827 ) ;
#6617 = AXIS2_PLACEMENT_3D ( 'NONE', #200, #6458, #8775 ) ;
#6618 = ORIENTED_EDGE ( 'NONE', *, *, #11873, .F. ) ;
#6619 = AXIS2_PLACEMENT_3D ( 'NONE', #12269, #6058, #4953 ) ;
#6620 = EDGE_CURVE ( 'NONE', #10761, #11792, #6395, .T. ) ;
#6621 = CARTESIAN_POINT ( 'NONE',  ( 0.000000000000000000, 0.000000000000000000, 0.000000000000000000 ) ) ;
#6622 = SURFACE_STYLE_FILL_AREA ( #569 ) ;
#6623 = DIRECTION ( 'NONE',  ( -0.000000000000000000, -1.000000000000000000, -0.000000000000000000 ) ) ;
#6624 = CARTESIAN_POINT ( 'NONE',  ( 6.000000000000008882, 3.000000000000000000, 27.00000000000000000 ) ) ;
#6625 = FACE_OUTER_BOUND ( 'NONE', #6127, .T. ) ;
#6626 = CARTESIAN_POINT ( 'NONE',  ( 0.000000000000000000, 1.000000000000000000, 0.000000000000000000 ) ) ;
#6627 = CARTESIAN_POINT ( 'NONE',  ( -4.174571361198896824, 9.000000000000000000, 6.065330394303907191 ) ) ;
#6628 = ORIENTED_EDGE ( 'NONE', *, *, #1343, .F. ) ;
#6629 = DIRECTION ( 'NONE',  ( 0.000000000000000000, 1.000000000000000000, -0.000000000000000000 ) ) ;
#6630 = ORIENTED_EDGE ( 'NONE', *, *, #6101, .T. ) ;
#6631 = VERTEX_POINT ( 'NONE', #13121 ) ;
#6632 = ORIENTED_EDGE ( 'NONE', *, *, #10323, .F. ) ;
#6633 = B_SPLINE_SURFACE_WITH_KNOTS ( 'NONE', 3, 1, ( 
 ( #12481, #71 ),
 ( #9561, #3019 ),
 ( #7226, #7487 ),
 ( #11691, #2182 ) ),
 .UNSPECIFIED., .F., .F., .F.,
 ( 4, 4 ),
 ( 2, 2 ),
 ( 0.000000000000000000, 0.8452273900860258760 ),
 ( 0.000000000000000000, 1.000000000000000000 ),
 .UNSPECIFIED. ) ;
#6634 = CARTESIAN_POINT ( 'NONE',  ( -0.8776997859584816375, 9.000000000000000000, 7.310603390113379341 ) ) ;
#6635 = CARTESIAN_POINT ( 'NONE',  ( 2.999999999999995559, 0.000000000000000000, -10.00000000000000355 ) ) ;
#6636 = CIRCLE ( 'NONE', #10157, 8.500000000000000000 ) ;
#6637 = ITEM_DEFINED_TRANSFORMATION ( 'NONE', 'NONE', #6283,  #10007 ) ;
#6638 = CARTESIAN_POINT ( 'NONE',  ( -8.479748006907129820, 9.000000000000000000, 0.5864074857593144507 ) ) ;
#6639 = LINE ( 'NONE', #2375, #9005 ) ;
#6640 = CARTESIAN_POINT ( 'NONE',  ( -10.18979803820068675, 0.000000000000000000, 6.506620931068438196 ) ) ;
#6641 = DIRECTION ( 'NONE',  ( -0.000000000000000000, -1.000000000000000000, 0.000000000000000000 ) ) ;
#6642 = ORIENTED_EDGE ( 'NONE', *, *, #9370, .F. ) ;
#6643 = AXIS2_PLACEMENT_3D ( 'NONE', #2177, #10854, #4242 ) ;
#6644 = ORIENTED_EDGE ( 'NONE', *, *, #8508, .T. ) ;
#6645 = VECTOR ( 'NONE', #10823, 1000.000000000000000 ) ;
#6646 = DIRECTION ( 'NONE',  ( 1.000000000000000000, 0.000000000000000000, 1.224646799147353207E-16 ) ) ;
#6647 = EDGE_CURVE ( 'NONE', #10019, #9707, #10082, .T. ) ;
#6648 = EDGE_CURVE ( 'NONE', #8949, #97, #11259, .T. ) ;
#6649 = B_SPLINE_SURFACE_WITH_KNOTS ( 'NONE', 3, 1, ( 
 ( #7326, #4018 ),
 ( #6352, #11529 ),
 ( #2093, #1056 ),
 ( #5253, #3189 ) ),
 .UNSPECIFIED., .F., .F., .F.,
 ( 4, 4 ),
 ( 2, 2 ),
 ( 0.1276832474596248101, 1.000000000000000000 ),
 ( 0.000000000000000000, 1.000000000000000000 ),
 .UNSPECIFIED. ) ;
#6650 = VERTEX_POINT ( 'NONE', #7944 ) ;
#6651 = DIRECTION ( 'NONE',  ( 0.000000000000000000, 1.000000000000000000, -0.000000000000000000 ) ) ;
#6652 = CARTESIAN_POINT ( 'NONE',  ( -6.017756925049793537, 3.000000000000000000, -11.52330688609026232 ) ) ;
#6653 = AXIS2_PLACEMENT_3D ( 'NONE', #5109, #7315, #10418 ) ;
#6654 = CYLINDRICAL_SURFACE ( 'NONE', #10175, 0.1000000000000000472 ) ;
#6655 = AXIS2_PLACEMENT_3D ( 'NONE', #532, #6784, #2524 ) ;
#6656 = AXIS2_PLACEMENT_3D ( 'NONE', #3037, #2978, #10415 ) ;
#6657 = CARTESIAN_POINT ( 'NONE',  ( 49.72134184781355515, 3.000000000000000000, -3.261665100124877981 ) ) ;
#6658 = CARTESIAN_POINT ( 'NONE',  ( 11.13895890373327724, 0.000000000000000000, -7.723663868796764476 ) ) ;
#6659 = CARTESIAN_POINT ( 'NONE',  ( 6.530577460941774603, 0.000000000000000000, 3.402183248810843885 ) ) ;
#6660 = CARTESIAN_POINT ( 'NONE',  ( -5.571433138827826426, 3.000000000000000000, -10.72973591378220526 ) ) ;
#6661 = DIRECTION ( 'NONE',  ( 0.000000000000000000, 0.000000000000000000, -1.000000000000000000 ) ) ;
#6662 = ORIENTED_EDGE ( 'NONE', *, *, #12071, .T. ) ;
#6663 = ADVANCED_FACE ( 'NONE', ( #11048 ), #3815, .F. ) ;
#6664 = EDGE_LOOP ( 'NONE', ( #9775, #9827, #13467, #6065 ) ) ;
#6665 = ADVANCED_FACE ( 'NONE', ( #8018, #12238, #8088, #12164, #6845, #2712, #1549, #13184, #1622, #6992 ), #724, .F. ) ;
#6666 = EDGE_LOOP ( 'NONE', ( #4852, #430 ) ) ;
#6667 = AXIS2_PLACEMENT_3D ( 'NONE', #11430, #968, #5093 ) ;
#6668 = VERTEX_POINT ( 'NONE', #4920 ) ;
#6669 = CYLINDRICAL_SURFACE ( 'NONE', #12404, 2.999999999999999112 ) ;
#6670 = TOROIDAL_SURFACE ( 'NONE', #13041, 1.600000000000004086, 0.1000000000000000056 ) ;
#6671 = AXIS2_PLACEMENT_3D ( 'NONE', #689, #7780, #9078 ) ;
#6672 = ORIENTED_EDGE ( 'NONE', *, *, #8385, .T. ) ;
#6673 = EDGE_CURVE ( 'NONE', #9781, #4442, #9193, .T. ) ;
#6674 = EDGE_CURVE ( 'NONE', #7910, #3196, #12305, .T. ) ;
#6675 = B_SPLINE_CURVE_WITH_KNOTS ( 'NONE', 3,
 ( #5147, #8167, #4043, #8107 ),
 .UNSPECIFIED., .F., .F.,
 ( 4, 4 ),
 ( 0.000000000000000000, 0.8724294488011776760 ),
 .UNSPECIFIED. ) ;
#6676 = FACE_BOUND ( 'NONE', #3101, .T. ) ;
#6677 = CARTESIAN_POINT ( 'NONE',  ( -9.600126836553261711, 0.000000000000000000, -8.482622935103767858 ) ) ;
#6678 = VECTOR ( 'NONE', #256, 1000.000000000000000 ) ;
#6679 = CARTESIAN_POINT ( 'NONE',  ( -4.334442004268530546, 9.000000000000000000, 7.311813216407585081 ) ) ;
#6680 = TOROIDAL_SURFACE ( 'NONE', #8857, 3.399999999999999911, 0.1000000000000000056 ) ;
#6681 = CARTESIAN_POINT ( 'NONE',  ( 9.250000000000001776, 2.000000000000000000, -10.00000000000000178 ) ) ;
#6682 = CARTESIAN_POINT ( 'NONE',  ( -12.40340517008309185, 0.000000000000000000, -3.893011711613028947 ) ) ;
#6683 = VERTEX_POINT ( 'NONE', #9937 ) ;
#6684 = DIRECTION ( 'NONE',  ( -0.000000000000000000, -1.000000000000000000, -0.000000000000000000 ) ) ;
#6685 = ORIENTED_EDGE ( 'NONE', *, *, #11824, .T. ) ;
#6686 = PRODUCT_DEFINITION_CONTEXT ( 'detailed design', #10569, 'design' ) ;
#6687 = ORIENTED_EDGE ( 'NONE', *, *, #3634, .F. ) ;
#6688 = CARTESIAN_POINT ( 'NONE',  ( 0.000000000000000000, 0.000000000000000000, 0.000000000000000000 ) ) ;
#6689 = ORIENTED_EDGE ( 'NONE', *, *, #7250, .F. ) ;
#6690 = AXIS2_PLACEMENT_3D ( 'NONE', #1636, #2792, #1840 ) ;
#6691 = AXIS2_PLACEMENT_3D ( 'NONE', #7657, #1321, #5516 ) ;
#6692 = ORIENTED_EDGE ( 'NONE', *, *, #6200, .T. ) ;
#6693 = DIRECTION ( 'NONE',  ( -3.469446951953614189E-15, -1.000000000000000000, 0.000000000000000000 ) ) ;
#6694 = DIRECTION ( 'NONE',  ( 0.000000000000000000, 0.000000000000000000, 1.000000000000000000 ) ) ;
#6695 = SURFACE_SIDE_STYLE ('',( #4619 ) ) ;
#6696 = LINE ( 'NONE', #8685, #10217 ) ;
#6697 = DIRECTION ( 'NONE',  ( -0.000000000000000000, -1.000000000000000000, -0.000000000000000000 ) ) ;
#6698 = DIRECTION ( 'NONE',  ( 0.000000000000000000, 0.000000000000000000, -1.000000000000000000 ) ) ;
#6699 = ORIENTED_EDGE ( 'NONE', *, *, #1401, .F. ) ;
#6700 = CARTESIAN_POINT ( 'NONE',  ( 6.970598036433451661, 0.000000000000000000, -10.97318381393796294 ) ) ;
#6701 = VECTOR ( 'NONE', #12122, 1000.000000000000000 ) ;
#6702 = EDGE_CURVE ( 'NONE', #5887, #12205, #2880, .T. ) ;
#6703 = ORIENTED_EDGE ( 'NONE', *, *, #12040, .F. ) ;
#6704 = VERTEX_POINT ( 'NONE', #12570 ) ;
#6705 = VERTEX_POINT ( 'NONE', #4215 ) ;
#6706 = CARTESIAN_POINT ( 'NONE',  ( 0.5398653231797245766, 3.000000000000000000, -12.07794044664754018 ) ) ;
#6707 = COLOUR_RGB ( '',0.7803921568627451011, 0.7607843137254901578, 0.7411764705882353255 ) ;
#6708 = AXIS2_PLACEMENT_3D ( 'NONE', #3590, #12907, #2362 ) ;
#6709 = CARTESIAN_POINT ( 'NONE',  ( -13.49999999999999645, 3.000000000000000000, -8.549999999999998934 ) ) ;
#6710 = CYLINDRICAL_SURFACE ( 'NONE', #443, 14.25000000000000178 ) ;
#6711 = FACE_OUTER_BOUND ( 'NONE', #12577, .T. ) ;
#6712 = DIRECTION ( 'NONE',  ( -0.000000000000000000, -1.000000000000000000, -0.000000000000000000 ) ) ;
#6713 = CARTESIAN_POINT ( 'NONE',  ( 0.000000000000000000, 2.900000000000000355, 0.000000000000000000 ) ) ;
#6714 = CARTESIAN_POINT ( 'NONE',  ( 0.8327827707325454742, 9.000000000000000000, 6.698430626405788679 ) ) ;
#6715 = ORIENTED_EDGE ( 'NONE', *, *, #2047, .F. ) ;
#6716 = TOROIDAL_SURFACE ( 'NONE', #8472, 1.600000000000000311, 0.1000000000000000056 ) ;
#6717 = ORIENTED_EDGE ( 'NONE', *, *, #1655, .F. ) ;
#6718 = VERTEX_POINT ( 'NONE', #4990 ) ;
#6719 = CARTESIAN_POINT ( 'NONE',  ( -8.158551673544284455, 0.000000000000000000, 8.922226997226891498 ) ) ;
#6720 = CARTESIAN_POINT ( 'NONE',  ( -14.82803603298498629, 0.000000000000000000, 2.264806262023049577 ) ) ;
#6721 =( GEOMETRIC_REPRESENTATION_CONTEXT ( 3 ) GLOBAL_UNCERTAINTY_ASSIGNED_CONTEXT ( ( #1868 ) ) GLOBAL_UNIT_ASSIGNED_CONTEXT ( ( #9482, #9281, #9359 ) ) REPRESENTATION_CONTEXT ( 'NONE', 'WORKASPACE' ) );
#6722 = FACE_OUTER_BOUND ( 'NONE', #1402, .T. ) ;
#6723 = CARTESIAN_POINT ( 'NONE',  ( 0.000000000000000000, -3.000000000000000000, 0.000000000000000000 ) ) ;
#6724 = CARTESIAN_POINT ( 'NONE',  ( 10.18979803820051622, 0.000000000000000000, -6.506620931068703761 ) ) ;
#6725 = EDGE_CURVE ( 'NONE', #523, #4083, #7399, .T. ) ;
#6726 = PRODUCT_RELATED_PRODUCT_CATEGORY ( 'part', '', ( #7531 ) ) ;
#6727 = CARTESIAN_POINT ( 'NONE',  ( 12.46219022525837694, 3.000000000000000000, -4.344528055836598845 ) ) ;
#6728 = LINE ( 'NONE', #2800, #4265 ) ;
#6729 = ORIENTED_EDGE ( 'NONE', *, *, #2283, .T. ) ;
#6730 = VERTEX_POINT ( 'NONE', #13537 ) ;
#6731 = VERTEX_POINT ( 'NONE', #2027 ) ;
#6732 = ORIENTED_EDGE ( 'NONE', *, *, #1342, .F. ) ;
#6733 = CARTESIAN_POINT ( 'NONE',  ( 31.00000000000000000, 0.000000000000000000, 0.000000000000000000 ) ) ;
#6734 = ORIENTED_EDGE ( 'NONE', *, *, #1796, .T. ) ;
#6735 = B_SPLINE_CURVE_WITH_KNOTS ( 'NONE', 3,
 ( #6364, #10572, #1135, #1540 ),
 .UNSPECIFIED., .F., .F.,
 ( 4, 4 ),
 ( 0.000000000000000000, 0.8724294488011777871 ),
 .UNSPECIFIED. ) ;
#6736 = CARTESIAN_POINT ( 'NONE',  ( 5.784789447945496654, 0.000000000000000000, -12.25836857253663581 ) ) ;
#6737 = ADVANCED_FACE ( 'NONE', ( #5121 ), #10430, .T. ) ;
#6738 = DIRECTION ( 'NONE',  ( 0.000000000000000000, 0.000000000000000000, 1.000000000000000000 ) ) ;
#6739 = CARTESIAN_POINT ( 'NONE',  ( -2.632142621505047408, 0.000000000000000000, -6.877144614729746586 ) ) ;
#6740 = ADVANCED_FACE ( 'NONE', ( #999 ), #13466, .F. ) ;
#6741 = CARTESIAN_POINT ( 'NONE',  ( 5.784789447945496654, 3.000000000000000000, -12.25836857253663581 ) ) ;
#6742 = CYLINDRICAL_SURFACE ( 'NONE', #11701, 14.24999999999999822 ) ;
#6743 = CARTESIAN_POINT ( 'NONE',  ( 6.017756925049591921, 3.000000000000000000, -11.52330688609011844 ) ) ;
#6744 = ORIENTED_EDGE ( 'NONE', *, *, #2114, .F. ) ;
#6745 = EDGE_CURVE ( 'NONE', #10193, #930, #5051, .T. ) ;
#6746 = CARTESIAN_POINT ( 'NONE',  ( -2.264806262022998062, 0.000000000000000000, -14.82803603298499340 ) ) ;
#6747 = EDGE_CURVE ( 'NONE', #1810, #9927, #8522, .T. ) ;
#6748 = VERTEX_POINT ( 'NONE', #11398 ) ;
#6749 = ORIENTED_EDGE ( 'NONE', *, *, #10044, .F. ) ;
#6750 = CARTESIAN_POINT ( 'NONE',  ( -14.82803603298498629, 3.000000000000000000, 2.264806262023049577 ) ) ;
#6751 = ORIENTED_EDGE ( 'NONE', *, *, #5721, .F. ) ;
#6752 = ORIENTED_EDGE ( 'NONE', *, *, #2483, .F. ) ;
#6753 = DIRECTION ( 'NONE',  ( -0.000000000000000000, -1.000000000000000000, -0.000000000000000000 ) ) ;
#6754 = CARTESIAN_POINT ( 'NONE',  ( 0.000000000000000000, 0.000000000000000000, 0.000000000000000000 ) ) ;
#6755 = CARTESIAN_POINT ( 'NONE',  ( -7.235926821844430812, 0.000000000000000000, 4.459973433655439301 ) ) ;
#6756 = ADVANCED_FACE ( 'NONE', ( #10355 ), #3191, .F. ) ;
#6757 = CARTESIAN_POINT ( 'NONE',  ( 9.375397774054407662, 0.000000000000000000, -11.70905276178460497 ) ) ;
#6758 = DIRECTION ( 'NONE',  ( -1.000000000000000000, 3.469446951953610639E-15, 2.602085213965210149E-16 ) ) ;
#6759 = DIRECTION ( 'NONE',  ( 0.000000000000000000, 0.000000000000000000, 1.000000000000000000 ) ) ;
#6760 = ORIENTED_EDGE ( 'NONE', *, *, #9429, .T. ) ;
#6761 = CARTESIAN_POINT ( 'NONE',  ( 7.500000000000004441, 0.000000000000000000, 21.89999999999999858 ) ) ;
#6762 = B_SPLINE_SURFACE_WITH_KNOTS ( 'NONE', 3, 1, ( 
 ( #9719, #7599 ),
 ( #7722, #6421 ),
 ( #4358, #2360 ),
 ( #11799, #9853 ) ),
 .UNSPECIFIED., .F., .F., .F.,
 ( 4, 4 ),
 ( 2, 2 ),
 ( 0.1547128134717859205, 1.000000000000000000 ),
 ( 0.000000000000000000, 1.000000000000000000 ),
 .UNSPECIFIED. ) ;
#6763 = EDGE_CURVE ( 'NONE', #3554, #12628, #8286, .T. ) ;
#6764 = ORIENTED_EDGE ( 'NONE', *, *, #10453, .T. ) ;
#6765 = ORIENTED_EDGE ( 'NONE', *, *, #8055, .T. ) ;
#6766 = B_SPLINE_CURVE_WITH_KNOTS ( 'NONE', 2,
 ( #7260, #8411, #5049 ),
 .UNSPECIFIED., .F., .F.,
 ( 3, 3 ),
 ( 0.000000000000000000, 1.000000000000000000 ),
 .UNSPECIFIED. ) ;
#6767 = VERTEX_POINT ( 'NONE', #9327 ) ;
#6768 = CARTESIAN_POINT ( 'NONE',  ( -7.939678587550617728, -1.694065894508600678E-18, 0.2057875656132798770 ) ) ;
#6769 = CARTESIAN_POINT ( 'NONE',  ( -1.650143266773857142, 3.000000000000000000, -14.90895795148409952 ) ) ;
#6770 = CARTESIAN_POINT ( 'NONE',  ( -8.504652361247167391, 3.000000000000000000, -9.593885948927674434 ) ) ;
#6771 = ADVANCED_FACE ( 'NONE', ( #9248 ), #9095, .T. ) ;
#6772 = ADVANCED_FACE ( 'NONE', ( #10231 ), #4745, .F. ) ;
#6773 = CARTESIAN_POINT ( 'NONE',  ( -4.190859029938718727, 0.000000000000000000, -6.054087828318142073 ) ) ;
#6774 = CONTEXT_DEPENDENT_SHAPE_REPRESENTATION ( #8182, #9535 ) ;
#6775 = DIRECTION ( 'NONE',  ( -0.000000000000000000, -1.000000000000000000, 0.000000000000000000 ) ) ;
#6776 = CARTESIAN_POINT ( 'NONE',  ( 0.000000000000000000, 0.000000000000000000, 0.000000000000000000 ) ) ;
#6777 = CARTESIAN_POINT ( 'NONE',  ( -2.481593227817846525, 9.000000000000000000, -8.129679886173168057 ) ) ;
#6778 = DIRECTION ( 'NONE',  ( 0.000000000000000000, 1.000000000000000000, -0.000000000000000000 ) ) ;
#6779 = ORIENTED_EDGE ( 'NONE', *, *, #6725, .T. ) ;
#6780 = ORIENTED_EDGE ( 'NONE', *, *, #6160, .T. ) ;
#6781 = ORIENTED_EDGE ( 'NONE', *, *, #2285, .T. ) ;
#6782 = DIRECTION ( 'NONE',  ( -0.000000000000000000, -1.000000000000000000, -0.000000000000000000 ) ) ;
#6783 = CYLINDRICAL_SURFACE ( 'NONE', #5812, 3.000000000000000000 ) ;
#6784 = DIRECTION ( 'NONE',  ( -0.000000000000000000, -1.000000000000000000, -0.000000000000000000 ) ) ;
#6785 = DIRECTION ( 'NONE',  ( 0.000000000000000000, 0.000000000000000000, 1.000000000000000000 ) ) ;
#6786 = LINE ( 'NONE', #2729, #11234 ) ;
#6787 = CARTESIAN_POINT ( 'NONE',  ( 50.46378962010818015, 0.000000000000000000, -4.178819016005276943 ) ) ;
#6788 = FACE_OUTER_BOUND ( 'NONE', #8532, .T. ) ;
#6789 = CARTESIAN_POINT ( 'NONE',  ( 3.469446951953614189E-15, 3.000000000000000000, -20.55000000000000071 ) ) ;
#6790 = ORIENTED_EDGE ( 'NONE', *, *, #9935, .T. ) ;
#6791 = EDGE_LOOP ( 'NONE', ( #5765, #9062 ) ) ;
#6792 = ORIENTED_EDGE ( 'NONE', *, *, #12051, .F. ) ;
#6793 = PLANE ( 'NONE',  #7111 ) ;
#6794 = EDGE_CURVE ( 'NONE', #11616, #6718, #4093, .T. ) ;
#6795 = ORIENTED_EDGE ( 'NONE', *, *, #1359, .F. ) ;
#6796 = VECTOR ( 'NONE', #12808, 1000.000000000000000 ) ;
#6797 = CARTESIAN_POINT ( 'NONE',  ( 0.000000000000000000, 3.000000000000000000, 0.000000000000000000 ) ) ;
#6798 = FILL_AREA_STYLE ('',( #3428 ) ) ;
#6799 = CARTESIAN_POINT ( 'NONE',  ( -5.250000000000000000, 3.000000000000000000, -27.94078293894052578 ) ) ;
#6800 = LINE ( 'NONE', #10698, #13441 ) ;
#6801 = DIRECTION ( 'NONE',  ( 1.000000000000000000, -3.469446951953610639E-15, -2.602085213965210149E-16 ) ) ;
#6802 = CYLINDRICAL_SURFACE ( 'NONE', #5331, 2.999999999999992450 ) ;
#6803 = LINE ( 'NONE', #3569, #3408 ) ;
#6804 = ORIENTED_EDGE ( 'NONE', *, *, #11329, .F. ) ;
#6805 = FILL_AREA_STYLE ('',( #9907 ) ) ;
#6806 = VECTOR ( 'NONE', #11411, 1000.000000000000000 ) ;
#6807 = EDGE_LOOP ( 'NONE', ( #98, #3243 ) ) ;
#6808 = CIRCLE ( 'NONE', #13198, 2.999999999999999112 ) ;
#6809 = UNCERTAINTY_MEASURE_WITH_UNIT (LENGTH_MEASURE( 1.000000000000000082E-05 ), #10648, 'distance_accuracy_value', 'NONE');
#6810 = EDGE_LOOP ( 'NONE', ( #6468, #10111, #10297, #6979 ) ) ;
#6811 = CARTESIAN_POINT ( 'NONE',  ( -2.375523406013128724, 9.000000000000000000, 6.318179211409233886 ) ) ;
#6812 = EDGE_CURVE ( 'NONE', #11589, #3853, #11335, .T. ) ;
#6813 = EDGE_CURVE ( 'NONE', #9985, #2397, #12453, .T. ) ;
#6814 = ORIENTED_EDGE ( 'NONE', *, *, #8337, .T. ) ;
#6815 = VERTEX_POINT ( 'NONE', #7203 ) ;
#6816 = CARTESIAN_POINT ( 'NONE',  ( 11.11702303352196708, 0.000000000000000000, 8.914835885878218846 ) ) ;
#6817 = ADVANCED_FACE ( 'NONE', ( #3515 ), #11800, .T. ) ;
#6818 = AXIS2_PLACEMENT_3D ( 'NONE', #2198, #6399, #8527 ) ;
#6819 = CARTESIAN_POINT ( 'NONE',  ( 31.00000000000000000, 0.09999999999999982514, 0.000000000000000000 ) ) ;
#6820 = PRESENTATION_STYLE_ASSIGNMENT (( #8952 ) ) ;
#6821 = CIRCLE ( 'NONE', #2201, 12.08999999999737085 ) ;
#6822 = CARTESIAN_POINT ( 'NONE',  ( -12.78643498603817896, 0.000000000000000000, 0.7901945867173603144 ) ) ;
#6823 = CARTESIAN_POINT ( 'NONE',  ( 8.760376775873721655, 3.000000000000000000, -10.34346111134700585 ) ) ;
#6824 = CARTESIAN_POINT ( 'NONE',  ( 1.734723475976807094E-15, 2.000000000000000000, 7.000000000000000000 ) ) ;
#6825 = ORIENTED_EDGE ( 'NONE', *, *, #5889, .F. ) ;
#6826 = CARTESIAN_POINT ( 'NONE',  ( 6.079397157347990799, 9.000000000000000000, 5.110946565852551693 ) ) ;
#6827 = ORIENTED_EDGE ( 'NONE', *, *, #9593, .F. ) ;
#6828 = VERTEX_POINT ( 'NONE', #3388 ) ;
#6829 = CIRCLE ( 'NONE', #5508, 0.09999999999999982514 ) ;
#6830 = EDGE_CURVE ( 'NONE', #2029, #10193, #7601, .T. ) ;
#6831 = B_SPLINE_SURFACE_WITH_KNOTS ( 'NONE', 2, 1, ( 
 ( #207, #2398 ),
 ( #8928, #11281 ),
 ( #5692, #9966 ) ),
 .UNSPECIFIED., .F., .F., .F.,
 ( 3, 3 ),
 ( 2, 2 ),
 ( 0.000000000000000000, 1.000000000000000000 ),
 ( 0.000000000000000000, 1.000000000000000000 ),
 .UNSPECIFIED. ) ;
#6832 = AXIS2_PLACEMENT_3D ( 'NONE', #9071, #11423, #13290 ) ;
#6833 = EDGE_LOOP ( 'NONE', ( #3156, #11885, #12792, #12383 ) ) ;
#6834 = ADVANCED_FACE ( 'NONE', ( #5451 ), #3249, .F. ) ;
#6835 = DIRECTION ( 'NONE',  ( 0.000000000000000000, 0.000000000000000000, -1.000000000000000000 ) ) ;
#6836 = EDGE_CURVE ( 'NONE', #3870, #10809, #6560, .T. ) ;
#6837 = CARTESIAN_POINT ( 'NONE',  ( 0.000000000000000000, 9.000000000000000000, 0.000000000000000000 ) ) ;
#6838 = EDGE_CURVE ( 'NONE', #9675, #5777, #3991, .T. ) ;
#6839 = CARTESIAN_POINT ( 'NONE',  ( -6.970598036433426792, 3.000000000000000000, -10.97318381393771780 ) ) ;
#6840 = CARTESIAN_POINT ( 'NONE',  ( -10.72973591378220348, 0.000000000000000000, 5.571433138827830867 ) ) ;
#6841 = LINE ( 'NONE', #4711, #8785 ) ;
#6842 = CARTESIAN_POINT ( 'NONE',  ( -14.16466328168010769, 3.000000000000000000, -1.557181465540673271 ) ) ;
#6843 = TOROIDAL_SURFACE ( 'NONE', #7715, 3.400000000000001243, 0.1000000000000000056 ) ;
#6844 = DIRECTION ( 'NONE',  ( 0.7216024245882196597, 0.000000000000000000, -0.6923076923076926237 ) ) ;
#6845 = FACE_OUTER_BOUND ( 'NONE', #5361, .T. ) ;
#6846 = AXIS2_PLACEMENT_3D ( 'NONE', #12918, #9736, #3465 ) ;
#6847 = CARTESIAN_POINT ( 'NONE',  ( 10.18979803820052155, 0.000000000000000000, -6.506620931068708202 ) ) ;
#6848 = PLANE ( 'NONE',  #13265 ) ;
#6849 = ORIENTED_EDGE ( 'NONE', *, *, #8272, .F. ) ;
#6850 = ORIENTED_EDGE ( 'NONE', *, *, #3263, .F. ) ;
#6851 = AXIS2_PLACEMENT_3D ( 'NONE', #8899, #13044, #6835 ) ;
#6852 = VECTOR ( 'NONE', #1903, 1000.000000000000000 ) ;
#6853 = ORIENTED_EDGE ( 'NONE', *, *, #4470, .T. ) ;
#6854 = CARTESIAN_POINT ( 'NONE',  ( 12.25282671965375592, 0.000000000000000000, -5.797378255456012930 ) ) ;
#6855 = DIRECTION ( 'NONE',  ( -0.000000000000000000, -1.000000000000000000, 0.000000000000000000 ) ) ;
#6856 = CARTESIAN_POINT ( 'NONE',  ( -8.158651161643904359, 0.000000000000000000, -8.922136023539605887 ) ) ;
#6857 = CARTESIAN_POINT ( 'NONE',  ( 26.30958424017656938, 2.900000000000000355, -4.500000000000000888 ) ) ;
#6858 = CARTESIAN_POINT ( 'NONE',  ( -12.56087513340552242, 3.000000000000000000, 2.568302020731519253 ) ) ;
#6859 = CARTESIAN_POINT ( 'NONE',  ( -8.222660081691577361, 0.000000000000000000, -5.549999999999999822 ) ) ;
#6860 = AXIS2_PLACEMENT_3D ( 'NONE', #2377, #442, #5407 ) ;
#6861 = DIRECTION ( 'NONE',  ( 0.000000000000000000, 1.000000000000000000, 0.000000000000000000 ) ) ;
#6862 = FACE_OUTER_BOUND ( 'NONE', #2300, .T. ) ;
#6863 = ORIENTED_EDGE ( 'NONE', *, *, #11909, .T. ) ;
#6864 = EDGE_CURVE ( 'NONE', #7415, #205, #13149, .T. ) ;
#6865 = EDGE_LOOP ( 'NONE', ( #4689, #1591, #8852, #6562 ) ) ;
#6866 = ADVANCED_FACE ( 'NONE', ( #1125 ), #3389, .T. ) ;
#6867 = VERTEX_POINT ( 'NONE', #1322 ) ;
#6868 = CARTESIAN_POINT ( 'NONE',  ( -1.604252589105048976, 9.000000000000000000, -8.347237484961699039 ) ) ;
#6869 = ORIENTED_EDGE ( 'NONE', *, *, #6327, .T. ) ;
#6870 = AXIS2_PLACEMENT_3D ( 'NONE', #12629, #3302, #12698 ) ;
#6871 = CIRCLE ( 'NONE', #4885, 1.500000000000000666 ) ;
#6872 = AXIS2_PLACEMENT_3D ( 'NONE', #9660, #7726, #1471 ) ;
#6873 = DIRECTION ( 'NONE',  ( 0.000000000000000000, 0.000000000000000000, 1.000000000000000000 ) ) ;
#6874 = CARTESIAN_POINT ( 'NONE',  ( 5.727824870043872529, 31.33135765298363040, -11.34110233529575140 ) ) ;
#6875 = CARTESIAN_POINT ( 'NONE',  ( 2.719999999999997087, 2.000000000000000000, -7.500000000000000000 ) ) ;
#6876 = DIRECTION ( 'NONE',  ( 0.000000000000000000, 0.000000000000000000, 1.000000000000000000 ) ) ;
#6877 = CARTESIAN_POINT ( 'NONE',  ( 12.00000000000000000, 2.749999999999992006, -10.00000000000000178 ) ) ;
#6878 = DIRECTION ( 'NONE',  ( -0.000000000000000000, -1.000000000000000000, -0.000000000000000000 ) ) ;
#6879 = CARTESIAN_POINT ( 'NONE',  ( 30.66173999750687784, 3.000000000000000000, 0.01003121477750366919 ) ) ;
#6880 = ORIENTED_EDGE ( 'NONE', *, *, #9876, .F. ) ;
#6881 = AXIS2_PLACEMENT_3D ( 'NONE', #1163, #5291, #10600 ) ;
#6882 = VECTOR ( 'NONE', #2169, 1000.000000000000227 ) ;
#6883 = AXIS2_PLACEMENT_3D ( 'NONE', #10277, #6341, #7119 ) ;
#6884 = ORIENTED_EDGE ( 'NONE', *, *, #197, .F. ) ;
#6885 = EDGE_LOOP ( 'NONE', ( #7856, #6685 ) ) ;
#6886 = CARTESIAN_POINT ( 'NONE',  ( -7.065816209474154341, 3.000000000000000000, 10.69794375946289833 ) ) ;
#6887 = ORIENTED_EDGE ( 'NONE', *, *, #10469, .F. ) ;
#6888 = CARTESIAN_POINT ( 'NONE',  ( -8.100301009650799244, 0.000000000000000000, -2.575873357339268033 ) ) ;
#6889 = EDGE_LOOP ( 'NONE', ( #4833, #12456, #10038, #4122 ) ) ;
#6890 = CARTESIAN_POINT ( 'NONE',  ( -13.03533457366735426, 3.000000000000000000, -6.217402469309218027 ) ) ;
#6891 = AXIS2_PLACEMENT_3D ( 'NONE', #7946, #12165, #12306 ) ;
#6892 = AXIS2_PLACEMENT_3D ( 'NONE', #6150, #8483, #10353 ) ;
#6893 = VECTOR ( 'NONE', #10376, 1000.000000000000000 ) ;
#6894 = CARTESIAN_POINT ( 'NONE',  ( -5.977417671213807182, 1.734723475976807094E-15, 3.135757960025121527 ) ) ;
#6895 =( LENGTH_UNIT ( ) NAMED_UNIT ( * ) SI_UNIT ( .MILLI., .METRE. ) );
#6896 = CARTESIAN_POINT ( 'NONE',  ( -3.188443695493920593, 0.000000000000000000, -12.60833606734848189 ) ) ;
#6897 = LINE ( 'NONE', #5868, #9272 ) ;
#6898 = CARTESIAN_POINT ( 'NONE',  ( 0.000000000000000000, 0.000000000000000000, 0.000000000000000000 ) ) ;
#6899 = EDGE_CURVE ( 'NONE', #3720, #11537, #7401, .T. ) ;
#6900 = ORIENTED_EDGE ( 'NONE', *, *, #2101, .F. ) ;
#6901 = CARTESIAN_POINT ( 'NONE',  ( 5.051606143860416509, 9.000000000000000000, 4.477027514692274224 ) ) ;
#6902 = ORIENTED_EDGE ( 'NONE', *, *, #8337, .F. ) ;
#6903 = VERTEX_POINT ( 'NONE', #9721 ) ;
#6904 = AXIS2_PLACEMENT_3D ( 'NONE', #9918, #5794, #1598 ) ;
#6905 = CARTESIAN_POINT ( 'NONE',  ( -4.334442004268530546, 0.000000000000000000, 7.311813216407585081 ) ) ;
#6906 = CIRCLE ( 'NONE', #12847, 3.399999999999999911 ) ;
#6907 = EDGE_LOOP ( 'NONE', ( #13281, #5582, #9219, #2411 ) ) ;
#6908 = DIRECTION ( 'NONE',  ( 0.000000000000000000, 0.000000000000000000, 1.000000000000000000 ) ) ;
#6909 = DIRECTION ( 'NONE',  ( 1.055752450943286467E-16, -0.000000000000000000, 1.000000000000000000 ) ) ;
#6910 = CARTESIAN_POINT ( 'NONE',  ( 53.78299299645824050, 3.000000000000000000, -4.528231303176834643 ) ) ;
#6911 = CARTESIAN_POINT ( 'NONE',  ( 0.000000000000000000, 3.000000000000000000, 0.000000000000000000 ) ) ;
#6912 = B_SPLINE_CURVE_WITH_KNOTS ( 'NONE', 3,
 ( #6968, #13439, #9013, #3992 ),
 .UNSPECIFIED., .F., .F.,
 ( 4, 4 ),
 ( 0.000000000000000000, 0.8452273900860258760 ),
 .UNSPECIFIED. ) ;
#6913 = FACE_OUTER_BOUND ( 'NONE', #7106, .T. ) ;
#6914 = CIRCLE ( 'NONE', #6690, 1.000000000000000888 ) ;
#6915 = DIRECTION ( 'NONE',  ( 0.000000000000000000, 0.000000000000000000, 1.000000000000000000 ) ) ;
#6916 = CIRCLE ( 'NONE', #1423, 1.500000000000000222 ) ;
#6917 = EDGE_CURVE ( 'NONE', #9840, #1800, #10023, .T. ) ;
#6918 = DIRECTION ( 'NONE',  ( 0.000000000000000000, 1.000000000000000000, 0.000000000000000000 ) ) ;
#6919 = CARTESIAN_POINT ( 'NONE',  ( -7.798201703419567643, 3.000000000000000000, -27.99999999999999289 ) ) ;
#6920 = EDGE_CURVE ( 'NONE', #3087, #9002, #5413, .T. ) ;
#6921 = LINE ( 'NONE', #9185, #2264 ) ;
#6922 = CARTESIAN_POINT ( 'NONE',  ( 31.00000000000000000, 3.000000000000000000, 3.999999998926329514 ) ) ;
#6923 = EDGE_LOOP ( 'NONE', ( #988, #982, #9557, #11719 ) ) ;
#6924 = ADVANCED_FACE ( 'NONE', ( #12963 ), #10562, .F. ) ;
#6925 = ORIENTED_EDGE ( 'NONE', *, *, #11069, .F. ) ;
#6926 = ADVANCED_FACE ( 'NONE', ( #9528 ), #109, .T. ) ;
#6927 = CIRCLE ( 'NONE', #7798, 3.399999999999999911 ) ;
#6928 = VECTOR ( 'NONE', #5248, 1000.000000000000000 ) ;
#6929 = EDGE_LOOP ( 'NONE', ( #10362, #7247, #12988, #8223 ) ) ;
#6930 = CARTESIAN_POINT ( 'NONE',  ( 5.731782959214990036, 0.000000000000000000, 11.46814821560793618 ) ) ;
#6931 = DIRECTION ( 'NONE',  ( 0.000000000000000000, 0.000000000000000000, -1.000000000000000000 ) ) ;
#6932 = CARTESIAN_POINT ( 'NONE',  ( -10.18987059060247624, 3.000000000000000000, -6.506507307819711095 ) ) ;
#6933 = B_SPLINE_CURVE_WITH_KNOTS ( 'NONE', 3,
 ( #9623, #7426, #6459, #335 ),
 .UNSPECIFIED., .F., .F.,
 ( 4, 4 ),
 ( 0.1547128134717859205, 1.000000000000000000 ),
 .UNSPECIFIED. ) ;
#6934 = EDGE_CURVE ( 'NONE', #10001, #9552, #1195, .T. ) ;
#6935 = CARTESIAN_POINT ( 'NONE',  ( 51.38094353598858532, 3.000000000000000000, -3.436371243710653722 ) ) ;
#6936 = LINE ( 'NONE', #2796, #5286 ) ;
#6937 = STYLED_ITEM ( 'NONE', ( #10202 ), #13452 ) ;
#6938 = CARTESIAN_POINT ( 'NONE',  ( 13.27898586450067242, 3.000000000000000000, -5.170206418547655502 ) ) ;
#6939 = VECTOR ( 'NONE', #3083, 1000.000000000000000 ) ;
#6940 = DIRECTION ( 'NONE',  ( -0.000000000000000000, -1.000000000000000000, -0.000000000000000000 ) ) ;
#6941 = CARTESIAN_POINT ( 'NONE',  ( 4.690415759823430619, 0.000000000000000000, -1.399999999999999911 ) ) ;
#6942 = ORIENTED_EDGE ( 'NONE', *, *, #5031, .T. ) ;
#6943 = EDGE_CURVE ( 'NONE', #4645, #4598, #7527, .T. ) ;
#6944 = ORIENTED_EDGE ( 'NONE', *, *, #9677, .F. ) ;
#6945 = ORIENTED_EDGE ( 'NONE', *, *, #303, .T. ) ;
#6946 = CARTESIAN_POINT ( 'NONE',  ( 11.65525440103098731, 0.000000000000000000, 2.142386537870793362 ) ) ;
#6947 = B_SPLINE_CURVE_WITH_KNOTS ( 'NONE', 3,
 ( #407, #1658, #10047, #1580 ),
 .UNSPECIFIED., .F., .F.,
 ( 4, 4 ),
 ( 0.000000000000000000, 0.8724294488011758997 ),
 .UNSPECIFIED. ) ;
#6948 = ORIENTED_EDGE ( 'NONE', *, *, #9769, .F. ) ;
#6949 =( GEOMETRIC_REPRESENTATION_CONTEXT ( 3 ) GLOBAL_UNCERTAINTY_ASSIGNED_CONTEXT ( ( #8737 ) ) GLOBAL_UNIT_ASSIGNED_CONTEXT ( ( #9898, #8662, #2401 ) ) REPRESENTATION_CONTEXT ( 'NONE', 'WORKASPACE' ) );
#6950 = CARTESIAN_POINT ( 'NONE',  ( -2.568302020731516588, 3.000000000000000000, -12.56087513340552242 ) ) ;
#6951 = DIRECTION ( 'NONE',  ( 0.000000000000000000, 0.000000000000000000, 1.000000000000000000 ) ) ;
#6952 = EDGE_CURVE ( 'NONE', #1933, #9046, #11175, .T. ) ;
#6953 = DIRECTION ( 'NONE',  ( -0.6291930273683253860, 0.000000000000000000, 0.7772490812545754801 ) ) ;
#6954 = CARTESIAN_POINT ( 'NONE',  ( 28.56494132578241008, 3.000000000000000000, -0.9541491613812155270 ) ) ;
#6955 = EDGE_CURVE ( 'NONE', #1864, #10087, #6496, .T. ) ;
#6956 = CARTESIAN_POINT ( 'NONE',  ( 5.571313494980132397, 3.000000000000000000, -10.72979803820131472 ) ) ;
#6957 = CARTESIAN_POINT ( 'NONE',  ( 4.690415759823430619, 0.09999999999999982514, -4.500000000000000888 ) ) ;
#6958 = CARTESIAN_POINT ( 'NONE',  ( 2.568302020731520141, 0.000000000000000000, 12.56087513340552420 ) ) ;
#6959 = ORIENTED_EDGE ( 'NONE', *, *, #8463, .F. ) ;
#6960 = PRODUCT_DEFINITION_FORMATION_WITH_SPECIFIED_SOURCE ( 'ANY', '', #1263, .NOT_KNOWN. ) ;
#6961 = ORIENTED_EDGE ( 'NONE', *, *, #9677, .T. ) ;
#6962 = UNCERTAINTY_MEASURE_WITH_UNIT (LENGTH_MEASURE( 1.000000000000000082E-05 ), #2357, 'distance_accuracy_value', 'NONE');
#6963 = ORIENTED_EDGE ( 'NONE', *, *, #1901, .F. ) ;
#6964 = CARTESIAN_POINT ( 'NONE',  ( -2.590203375110137873, 9.000000000000000000, 6.893050072893555758 ) ) ;
#6965 = EDGE_LOOP ( 'NONE', ( #4, #5037, #12699, #5630 ) ) ;
#6966 = DIRECTION ( 'NONE',  ( -0.000000000000000000, -1.000000000000000000, -0.000000000000000000 ) ) ;
#6967 = ORIENTED_EDGE ( 'NONE', *, *, #12254, .T. ) ;
#6968 = CARTESIAN_POINT ( 'NONE',  ( -11.48836750521728689, 0.000000000000000000, -8.430890348300561499 ) ) ;
#6969 =( REPRESENTATION_RELATIONSHIP ('NONE','NONE', #3798, #11353 ) REPRESENTATION_RELATIONSHIP_WITH_TRANSFORMATION ( #6637 )SHAPE_REPRESENTATION_RELATIONSHIP( ) );
#6970 = CARTESIAN_POINT ( 'NONE',  ( 0.000000000000000000, 9.000000000000000000, 0.000000000000000000 ) ) ;
#6971 = CARTESIAN_POINT ( 'NONE',  ( -7.798201703419555209, 3.000000000000000000, -30.99999999999999289 ) ) ;
#6972 = DIRECTION ( 'NONE',  ( 0.000000000000000000, 0.000000000000000000, -1.000000000000000000 ) ) ;
#6973 = DIRECTION ( 'NONE',  ( -2.312964634635743450E-15, -1.000000000000000000, 0.000000000000000000 ) ) ;
#6974 = CARTESIAN_POINT ( 'NONE',  ( -1.557181465540760534, 0.000000000000000000, -14.16466328168009703 ) ) ;
#6975 = ORIENTED_EDGE ( 'NONE', *, *, #7064, .T. ) ;
#6976 = CARTESIAN_POINT ( 'NONE',  ( -6.025412986832177076, 0.000000000000000000, -13.73660796332610268 ) ) ;
#6977 = ORIENTED_EDGE ( 'NONE', *, *, #3411, .T. ) ;
#6978 = B_SPLINE_CURVE_WITH_KNOTS ( 'NONE', 3,
 ( #8195, #2827, #5999, #12429 ),
 .UNSPECIFIED., .F., .F.,
 ( 4, 4 ),
 ( 0.4545418633443863987, 0.4839599404020549223 ),
 .UNSPECIFIED. ) ;
#6979 = ORIENTED_EDGE ( 'NONE', *, *, #3044, .T. ) ;
#6980 = CARTESIAN_POINT ( 'NONE',  ( -1.105736515254454044, 3.000000000000000000, 13.50994833511691340 ) ) ;
#6981 = ORIENTED_EDGE ( 'NONE', *, *, #12742, .T. ) ;
#6982 = EDGE_CURVE ( 'NONE', #9461, #13528, #7867, .T. ) ;
#6983 = CARTESIAN_POINT ( 'NONE',  ( 2.525608486058770641, 2.900000000000000355, 2.423076923076923350 ) ) ;
#6984 = CARTESIAN_POINT ( 'NONE',  ( 9.573149624528804580, 3.000000000000000000, -8.795158114916638681 ) ) ;
#6985 = DIRECTION ( 'NONE',  ( 0.000000000000000000, 0.000000000000000000, 1.000000000000000000 ) ) ;
#6986 = CARTESIAN_POINT ( 'NONE',  ( 7.771282357155271825, 9.000000000000000000, -3.443424244174282389 ) ) ;
#6987 = DIRECTION ( 'NONE',  ( -0.9893737785712105604, -0.000000000000000000, 0.1453943818575021141 ) ) ;
#6988 = CONTEXT_DEPENDENT_SHAPE_REPRESENTATION ( #2301, #5235 ) ;
#6989 = CARTESIAN_POINT ( 'NONE',  ( 0.000000000000000000, 1.000000000000000000, 0.000000000000000000 ) ) ;
#6990 = B_SPLINE_SURFACE_WITH_KNOTS ( 'NONE', 3, 1, ( 
 ( #5974, #1855 ),
 ( #2743, #3845 ),
 ( #6950, #6055 ),
 ( #1652, #5844 ) ),
 .UNSPECIFIED., .F., .F., .F.,
 ( 4, 4 ),
 ( 2, 2 ),
 ( 0.000000000000000000, 0.8452273900860258760 ),
 ( 0.000000000000000000, 1.000000000000000000 ),
 .UNSPECIFIED. ) ;
#6991 = CARTESIAN_POINT ( 'NONE',  ( -7.077546079049271910, 0.000000000000000000, -10.67828022838850544 ) ) ;
#6992 = FACE_BOUND ( 'NONE', #4263, .T. ) ;
#6993 = CARTESIAN_POINT ( 'NONE',  ( 8.208497377870823897, 3.000000000000000000, -5.549999999999999822 ) ) ;
#6994 = LINE ( 'NONE', #5819, #9732 ) ;
#6995 = ORIENTED_EDGE ( 'NONE', *, *, #7677, .T. ) ;
#6996 = ORIENTED_EDGE ( 'NONE', *, *, #2101, .T. ) ;
#6997 = ORIENTED_EDGE ( 'NONE', *, *, #4725, .T. ) ;
#6998 = EDGE_CURVE ( 'NONE', #9688, #5557, #13242, .T. ) ;
#6999 = EDGE_CURVE ( 'NONE', #7580, #1090, #4763, .T. ) ;
#7000 = ORIENTED_EDGE ( 'NONE', *, *, #5220, .F. ) ;
#7001 = CARTESIAN_POINT ( 'NONE',  ( -8.760376775873710997, 3.000000000000000000, 10.34346111134700941 ) ) ;
#7002 = DIRECTION ( 'NONE',  ( -0.000000000000000000, -1.000000000000000000, -0.000000000000000000 ) ) ;
#7003 = CARTESIAN_POINT ( 'NONE',  ( -14.82803603298498629, 0.000000000000000000, 2.264806262023049577 ) ) ;
#7004 = ADVANCED_FACE ( 'NONE', ( #573 ), #7902, .T. ) ;
#7005 = FACE_OUTER_BOUND ( 'NONE', #7811, .T. ) ;
#7006 = CARTESIAN_POINT ( 'NONE',  ( 7.110882674384088276, 9.000000000000000000, -3.538387050178523729 ) ) ;
#7007 = CARTESIAN_POINT ( 'NONE',  ( 5.250000000000000000, 3.000000000000000000, -27.94078293894052578 ) ) ;
#7008 = CYLINDRICAL_SURFACE ( 'NONE', #6470, 13.50000000000000178 ) ;
#7009 = CARTESIAN_POINT ( 'NONE',  ( -1.105736515254454044, 0.000000000000000000, 13.50994833511691340 ) ) ;
#7010 = ORIENTED_EDGE ( 'NONE', *, *, #11211, .F. ) ;
#7011 = ORIENTED_EDGE ( 'NONE', *, *, #3662, .F. ) ;
#7012 = VERTEX_POINT ( 'NONE', #9098 ) ;
#7013 = CARTESIAN_POINT ( 'NONE',  ( 1.958311002203130480, 0.000000000000000000, -14.87484884897977366 ) ) ;
#7014 = EDGE_CURVE ( 'NONE', #10663, #8766, #5930, .T. ) ;
#7015 = ORIENTED_EDGE ( 'NONE', *, *, #969, .T. ) ;
#7016 = CARTESIAN_POINT ( 'NONE',  ( -10.98198414889942676, 0.000000000000000000, -9.379342464487661957 ) ) ;
#7017 = DIRECTION ( 'NONE',  ( 0.5644961850934593350, 4.383283236518789377E-16, -0.8254356770911533969 ) ) ;
#7018 = EDGE_CURVE ( 'NONE', #8307, #4532, #13238, .T. ) ;
#7019 = FACE_OUTER_BOUND ( 'NONE', #4977, .T. ) ;
#7020 = LINE ( 'NONE', #9973, #11901 ) ;
#7021 = DIRECTION ( 'NONE',  ( 0.000000000000000000, 1.000000000000000000, -0.000000000000000000 ) ) ;
#7022 = DIRECTION ( 'NONE',  ( -1.000000000000000000, -1.156482317317867583E-15, 0.000000000000000000 ) ) ;
#7023 = CARTESIAN_POINT ( 'NONE',  ( -0.8973464813148227526, 0.000000000000000000, -7.308217849399443189 ) ) ;
#7024 = ORIENTED_EDGE ( 'NONE', *, *, #2825, .T. ) ;
#7025 = CARTESIAN_POINT ( 'NONE',  ( 0.000000000000000000, 1.000000000000000000, 0.000000000000000000 ) ) ;
#7026 = ORIENTED_EDGE ( 'NONE', *, *, #1991, .F. ) ;
#7027 = EDGE_LOOP ( 'NONE', ( #6662, #12275, #12294, #3298 ) ) ;
#7028 = CARTESIAN_POINT ( 'NONE',  ( 11.59535436762926430, 0.000000000000000000, -5.877734009726468756 ) ) ;
#7029 = ADVANCED_FACE ( 'NONE', ( #3654 ), #2565, .T. ) ;
#7030 = EDGE_CURVE ( 'NONE', #2099, #12066, #2622, .T. ) ;
#7031 = EDGE_LOOP ( 'NONE', ( #12694, #2395, #6749, #9601 ) ) ;
#7032 = CARTESIAN_POINT ( 'NONE',  ( -6.025412986832177076, 0.000000000000000000, -13.73660796332610268 ) ) ;
#7033 = ORIENTED_EDGE ( 'NONE', *, *, #690, .T. ) ;
#7034 = CARTESIAN_POINT ( 'NONE',  ( 3.007863545083557355, 0.000000000000000000, 7.350755164602351677 ) ) ;
#7035 = DIRECTION ( 'NONE',  ( -0.6291930273683260522, 0.000000000000000000, 0.7772490812545750360 ) ) ;
#7036 = DIRECTION ( 'NONE',  ( -0.000000000000000000, -1.000000000000000000, -0.000000000000000000 ) ) ;
#7037 = CARTESIAN_POINT ( 'NONE',  ( 12.00000000000001421, 6.000000000000000000, -3.122502256758250009E-15 ) ) ;
#7038 = FACE_OUTER_BOUND ( 'NONE', #5594, .T. ) ;
#7039 = AXIS2_PLACEMENT_3D ( 'NONE', #7498, #2340, #7439 ) ;
#7040 = CARTESIAN_POINT ( 'NONE',  ( -20.56403552112892896, 3.000000000000000000, -16.70078978407140013 ) ) ;
#7041 = ORIENTED_EDGE ( 'NONE', *, *, #7746, .T. ) ;
#7042 = CARTESIAN_POINT ( 'NONE',  ( -6.329356821613726147, 0.000000000000000000, -12.30759122142001338 ) ) ;
#7043 = VERTEX_POINT ( 'NONE', #11170 ) ;
#7044 = VERTEX_POINT ( 'NONE', #9919 ) ;
#7045 = LINE ( 'NONE', #12441, #1377 ) ;
#7046 = ADVANCED_FACE ( 'NONE', ( #1601 ), #7080, .T. ) ;
#7047 = EDGE_CURVE ( 'NONE', #447, #4632, #6897, .T. ) ;
#7048 = ORIENTED_EDGE ( 'NONE', *, *, #5723, .F. ) ;
#7049 = AXIS2_PLACEMENT_3D ( 'NONE', #2508, #1545, #648 ) ;
#7050 = VECTOR ( 'NONE', #10011, 1000.000000000000227 ) ;
#7051 = CARTESIAN_POINT ( 'NONE',  ( 0.000000000000000000, 0.1000000000000000056, -1.399999999999999911 ) ) ;
#7052 = CARTESIAN_POINT ( 'NONE',  ( 9.593885948927676210, 0.000000000000000000, -8.504652361247169168 ) ) ;
#7053 = CARTESIAN_POINT ( 'NONE',  ( -8.914835885878284572, 0.000000000000000000, -11.11702303352191379 ) ) ;
#7054 = DIRECTION ( 'NONE',  ( 0.000000000000000000, 1.000000000000000000, -0.000000000000000000 ) ) ;
#7055 = DIRECTION ( 'NONE',  ( 0.000000000000000000, 1.000000000000000000, 0.000000000000000000 ) ) ;
#7056 = CARTESIAN_POINT ( 'NONE',  ( 9.133371500908369356, 3.000000000000000000, -11.90284147956862171 ) ) ;
#7057 = LINE ( 'NONE', #1692, #2662 ) ;
#7058 = DIRECTION ( 'NONE',  ( -0.000000000000000000, -1.000000000000000000, -0.000000000000000000 ) ) ;
#7059 = CARTESIAN_POINT ( 'NONE',  ( -0.5400000000007666445, 0.000000000000000000, -12.07793442604883793 ) ) ;
#7060 = CARTESIAN_POINT ( 'NONE',  ( 53.78299299645824050, 0.000000000000000000, -4.528231303176834643 ) ) ;
#7061 = VECTOR ( 'NONE', #10592, 1000.000000000000000 ) ;
#7062 = VECTOR ( 'NONE', #9524, 1000.000000000000000 ) ;
#7063 = ORIENTED_EDGE ( 'NONE', *, *, #3527, .F. ) ;
#7064 = EDGE_CURVE ( 'NONE', #5615, #6374, #12953, .T. ) ;
#7065 = ORIENTED_EDGE ( 'NONE', *, *, #3974, .T. ) ;
#7066 = EDGE_LOOP ( 'NONE', ( #12437, #3689, #3520, #5145 ) ) ;
#7067 = ORIENTED_EDGE ( 'NONE', *, *, #3782, .T. ) ;
#7068 = DIRECTION ( 'NONE',  ( -1.000000000000000000, 0.000000000000000000, 1.370446048119726253E-16 ) ) ;
#7069 = PRESENTATION_STYLE_ASSIGNMENT (( #735 ) ) ;
#7070 = CIRCLE ( 'NONE', #11683, 12.08999999999737440 ) ;
#7071 = CIRCLE ( 'NONE', #7930, 6.750000000000000888 ) ;
#7072 = DIRECTION ( 'NONE',  ( -0.000000000000000000, -1.000000000000000000, -0.000000000000000000 ) ) ;
#7073 = DIRECTION ( 'NONE',  ( 0.000000000000000000, 0.000000000000000000, 1.000000000000000000 ) ) ;
#7074 = CARTESIAN_POINT ( 'NONE',  ( 5.053288777954491273, 1.734723475976807094E-15, -4.475128213425755952 ) ) ;
#7075 = DIRECTION ( 'NONE',  ( -0.3802634127332040759, -0.000000000000000000, -0.9248782281665499649 ) ) ;
#7076 = ADVANCED_FACE ( 'NONE', ( #4828 ), #10833, .F. ) ;
#7077 = FACE_OUTER_BOUND ( 'NONE', #2759, .T. ) ;
#7078 = EDGE_CURVE ( 'NONE', #578, #6748, #9436, .T. ) ;
#7079 = ORIENTED_EDGE ( 'NONE', *, *, #7193, .F. ) ;
#7080 = TOROIDAL_SURFACE ( 'NONE', #10814, 1.600000000000000311, 0.1000000000000000056 ) ;
#7081 = DIRECTION ( 'NONE',  ( -0.000000000000000000, -1.000000000000000000, -0.000000000000000000 ) ) ;
#7082 = CARTESIAN_POINT ( 'NONE',  ( 0.000000000000000000, 9.000000000000000000, 0.000000000000000000 ) ) ;
#7083 = ORIENTED_EDGE ( 'NONE', *, *, #753, .F. ) ;
#7084 = CARTESIAN_POINT ( 'NONE',  ( 4.225031457058369317E-16, 0.000000000000000000, -3.400000000000001243 ) ) ;
#7085 = VECTOR ( 'NONE', #5203, 1000.000000000000000 ) ;
#7086 = CARTESIAN_POINT ( 'NONE',  ( -2.047579527507184860, 38.33135765298362685, 9.239060114367257270 ) ) ;
#7087 = AXIS2_PLACEMENT_3D ( 'NONE', #1483, #5611, #8762 ) ;
#7088 = CARTESIAN_POINT ( 'NONE',  ( 49.72134184781355515, 3.000000000000000000, -3.261665100124877981 ) ) ;
#7089 = CARTESIAN_POINT ( 'NONE',  ( 22.00000000000000000, 0.000000000000000000, -1.500000000000000666 ) ) ;
#7090 = CARTESIAN_POINT ( 'NONE',  ( -8.922136023539609440, 0.000000000000000000, 8.158651161643900807 ) ) ;
#7091 = ADVANCED_FACE ( 'NONE', ( #7038 ), #9499, .F. ) ;
#7092 = CARTESIAN_POINT ( 'NONE',  ( 46.02418392430381999, 3.000000000000000000, -15.41988256844266836 ) ) ;
#7093 = CARTESIAN_POINT ( 'NONE',  ( -11.35348746973813761, 3.000000000000000000, -6.343077501554963860 ) ) ;
#7094 = EDGE_CURVE ( 'NONE', #6748, #13415, #7307, .T. ) ;
#7095 = ORIENTED_EDGE ( 'NONE', *, *, #3705, .T. ) ;
#7096 = DIRECTION ( 'NONE',  ( 0.000000000000000000, 0.000000000000000000, -1.000000000000000000 ) ) ;
#7097 = ORIENTED_EDGE ( 'NONE', *, *, #596, .F. ) ;
#7098 = PRODUCT_DEFINITION_CONTEXT ( 'detailed design', #4404, 'design' ) ;
#7099 = ORIENTED_EDGE ( 'NONE', *, *, #6250, .T. ) ;
#7100 = VECTOR ( 'NONE', #9586, 1000.000000000000000 ) ;
#7101 = EDGE_CURVE ( 'NONE', #1063, #2645, #3996, .T. ) ;
#7102 = ORIENTED_EDGE ( 'NONE', *, *, #7677, .F. ) ;
#7103 = CARTESIAN_POINT ( 'NONE',  ( -3.533475733155565290, 9.000000000000000000, 7.730753471893975437 ) ) ;
#7104 = VECTOR ( 'NONE', #12903, 1000.000000000000000 ) ;
#7105 = EDGE_CURVE ( 'NONE', #3224, #12936, #11314, .T. ) ;
#7106 = EDGE_LOOP ( 'NONE', ( #10746, #6963, #9705, #7748 ) ) ;
#7107 = B_SPLINE_SURFACE_WITH_KNOTS ( 'NONE', 3, 1, ( 
 ( #12214, #3587 ),
 ( #11025, #4826 ),
 ( #9017, #1596 ),
 ( #571, #13234 ) ),
 .UNSPECIFIED., .F., .F., .F.,
 ( 4, 4 ),
 ( 2, 2 ),
 ( 0.1547128134717859205, 1.000000000000000000 ),
 ( 0.000000000000000000, 1.000000000000000000 ),
 .UNSPECIFIED. ) ;
#7108 = LINE ( 'NONE', #3786, #9857 ) ;
#7109 =( NAMED_UNIT ( * ) PLANE_ANGLE_UNIT ( ) SI_UNIT ( $, .RADIAN. ) );
#7110 = DIRECTION ( 'NONE',  ( 0.000000000000000000, 1.000000000000000000, 0.000000000000000000 ) ) ;
#7111 = AXIS2_PLACEMENT_3D ( 'NONE', #8043, #12264, #13078 ) ;
#7112 = DIRECTION ( 'NONE',  ( 0.000000000000000000, 0.000000000000000000, 1.000000000000000000 ) ) ;
#7113 = VECTOR ( 'NONE', #6044, 1000.000000000000227 ) ;
#7114 = AXIS2_PLACEMENT_3D ( 'NONE', #12968, #9858, #12708 ) ;
#7115 = ADVANCED_FACE ( 'NONE', ( #12433 ), #9167, .T. ) ;
#7116 = CARTESIAN_POINT ( 'NONE',  ( 8.795158114916441505, 3.000000000000000000, -9.573149624528689117 ) ) ;
#7117 = FACE_BOUND ( 'NONE', #11114, .T. ) ;
#7118 = ORIENTED_EDGE ( 'NONE', *, *, #3113, .F. ) ;
#7119 = DIRECTION ( 'NONE',  ( -0.7772490812545796990, 0.000000000000000000, -0.6291930273683203900 ) ) ;
#7120 = EDGE_LOOP ( 'NONE', ( #1399, #12562, #5782, #2485 ) ) ;
#7121 = EDGE_LOOP ( 'NONE', ( #13588, #3301, #8455, #12646 ) ) ;
#7122 = CARTESIAN_POINT ( 'NONE',  ( -2.632142621505047408, 9.000000000000000000, -6.877144614729746586 ) ) ;
#7123 = EDGE_LOOP ( 'NONE', ( #950, #9104 ) ) ;
#7124 = VECTOR ( 'NONE', #11131, 1000.000000000000000 ) ;
#7125 = VECTOR ( 'NONE', #12569, 1000.000000000000000 ) ;
#7126 = AXIS2_PLACEMENT_3D ( 'NONE', #3435, #6684, #7646 ) ;
#7127 = FACE_BOUND ( 'NONE', #7711, .T. ) ;
#7128 = CARTESIAN_POINT ( 'NONE',  ( 4.690415759823430619, 2.900000000000000355, 1.500000000000000000 ) ) ;
#7129 = CARTESIAN_POINT ( 'NONE',  ( 3.818534268238711782, 9.000000000000000000, -5.566084444408534004 ) ) ;
#7130 = LINE ( 'NONE', #6219, #8353 ) ;
#7131 = DIRECTION ( 'NONE',  ( -0.000000000000000000, -1.000000000000000000, -0.000000000000000000 ) ) ;
#7132 = CARTESIAN_POINT ( 'NONE',  ( 4.898587196589413075E-17, 0.000000000000000000, 0.4000000000000000222 ) ) ;
#7133 = EDGE_CURVE ( 'NONE', #12719, #3825, #5552, .T. ) ;
#7134 = CARTESIAN_POINT ( 'NONE',  ( -6.506620931068715308, 0.000000000000000000, -10.18979803820051799 ) ) ;
#7135 = DIRECTION ( 'NONE',  ( 0.7772490812545826966, 0.000000000000000000, 0.6291930273683166153 ) ) ;
#7136 = EDGE_CURVE ( 'NONE', #3491, #2253, #9486, .T. ) ;
#7137 = CIRCLE ( 'NONE', #1188, 1.500000000000003997 ) ;
#7138 = DIRECTION ( 'NONE',  ( 0.000000000000000000, 0.000000000000000000, -1.000000000000000000 ) ) ;
#7139 = CARTESIAN_POINT ( 'NONE',  ( 13.04554897075796838, 0.000000000000000000, -5.733772933379540859 ) ) ;
#7140 = CIRCLE ( 'NONE', #1189, 1.500000000000001332 ) ;
#7141 = ORIENTED_EDGE ( 'NONE', *, *, #1203, .F. ) ;
#7142 = VERTEX_POINT ( 'NONE', #5101 ) ;
#7143 = VERTEX_POINT ( 'NONE', #13380 ) ;
#7144 = VERTEX_POINT ( 'NONE', #12498 ) ;
#7145 = DIRECTION ( 'NONE',  ( 0.000000000000000000, 1.000000000000000000, 0.000000000000000000 ) ) ;
#7146 = VECTOR ( 'NONE', #1642, 1000.000000000000000 ) ;
#7147 = AXIS2_PLACEMENT_3D ( 'NONE', #8984, #13199, #12183 ) ;
#7148 = CARTESIAN_POINT ( 'NONE',  ( 10.72979803820131472, 0.000000000000000000, 5.571313494980131509 ) ) ;
#7149 = LINE ( 'NONE', #7881, #2258 ) ;
#7150 = CARTESIAN_POINT ( 'NONE',  ( 0.000000000000000000, 0.000000000000000000, 9.250000000000000000 ) ) ;
#7151 = CYLINDRICAL_SURFACE ( 'NONE', #3531, 9.250000000000000000 ) ;
#7152 = DIRECTION ( 'NONE',  ( 0.9100336346413741007, 0.000000000000000000, 0.4145344181384821858 ) ) ;
#7153 = AXIS2_PLACEMENT_3D ( 'NONE', #6837, #9865, #10009 ) ;
#7154 = DIRECTION ( 'NONE',  ( 0.000000000000000000, 1.000000000000000000, 0.000000000000000000 ) ) ;
#7155 = AXIS2_PLACEMENT_3D ( 'NONE', #7602, #304, #6759 ) ;
#7156 = ORIENTED_EDGE ( 'NONE', *, *, #5809, .F. ) ;
#7157 = DIRECTION ( 'NONE',  ( 0.000000000000000000, 0.000000000000000000, 1.000000000000000000 ) ) ;
#7158 = DIRECTION ( 'NONE',  ( -0.000000000000000000, -1.000000000000000000, -0.000000000000000000 ) ) ;
#7159 = ORIENTED_EDGE ( 'NONE', *, *, #10391, .T. ) ;
#7160 = ADVANCED_FACE ( 'NONE', ( #6270 ), #8388, .T. ) ;
#7161 = DIRECTION ( 'NONE',  ( -0.000000000000000000, -1.000000000000000000, -0.000000000000000000 ) ) ;
#7162 = MECHANICAL_DESIGN_GEOMETRIC_PRESENTATION_REPRESENTATION (  '', ( #9790 ), #7372 ) ;
#7163 = APPLICATION_PROTOCOL_DEFINITION ( 'draft international standard', 'automotive_design', 1998, #4143 ) ;
#7164 = CARTESIAN_POINT ( 'NONE',  ( -9.375397774054503586, 3.000000000000000000, -11.70905276178452503 ) ) ;
#7165 = CARTESIAN_POINT ( 'NONE',  ( 19.60942157306000766, 3.000000000000000000, 14.05941790610251374 ) ) ;
#7166 = DIRECTION ( 'NONE',  ( -1.000000000000000000, 0.000000000000000000, 0.000000000000000000 ) ) ;
#7167 = CARTESIAN_POINT ( 'NONE',  ( 9.249999999999996447, -1.734723475976807094E-15, -10.00000000000000355 ) ) ;
#7168 = CARTESIAN_POINT ( 'NONE',  ( 10.72979803820131472, 3.000000000000000000, 5.571313494980131509 ) ) ;
#7169 = CARTESIAN_POINT ( 'NONE',  ( 13.27898586450067420, 0.000000000000000000, 5.170206418547648397 ) ) ;
#7170 = VERTEX_POINT ( 'NONE', #1882 ) ;
#7171 = ORIENTED_EDGE ( 'NONE', *, *, #12605, .T. ) ;
#7172 = STYLED_ITEM ( 'NONE', ( #8727 ), #2434 ) ;
#7173 = ORIENTED_EDGE ( 'NONE', *, *, #4492, .T. ) ;
#7174 = CARTESIAN_POINT ( 'NONE',  ( 0.000000000000000000, 0.000000000000000000, -12.08999999999737440 ) ) ;
#7175 = VERTEX_POINT ( 'NONE', #7243 ) ;
#7176 = EDGE_CURVE ( 'NONE', #6069, #7533, #7302, .T. ) ;
#7177 = EDGE_CURVE ( 'NONE', #2682, #11250, #2008, .T. ) ;
#7178 = CARTESIAN_POINT ( 'NONE',  ( 2.620242232815953809, 9.000000000000000000, 6.881105251569436199 ) ) ;
#7179 = CARTESIAN_POINT ( 'NONE',  ( 7.758214145541979967, 9.000000000000000000, 1.700281702449083054 ) ) ;
#7180 = FILL_AREA_STYLE ('',( #8324 ) ) ;
#7181 = AXIS2_PLACEMENT_3D ( 'NONE', #3905, #13211, #10255 ) ;
#7182 = EDGE_CURVE ( 'NONE', #8454, #2033, #3768, .T. ) ;
#7183 = CARTESIAN_POINT ( 'NONE',  ( 13.04554897075798081, 3.000000000000000000, -5.733772933379503556 ) ) ;
#7184 = EDGE_CURVE ( 'NONE', #5027, #4139, #5178, .T. ) ;
#7185 = CARTESIAN_POINT ( 'NONE',  ( 9.375397774054407662, 0.000000000000000000, -11.70905276178460497 ) ) ;
#7186 = DIRECTION ( 'NONE',  ( -0.000000000000000000, -1.000000000000000000, -0.000000000000000000 ) ) ;
#7187 = EDGE_LOOP ( 'NONE', ( #1044, #6111, #255, #9127, #9249, #12773, #13301, #2981, #10733, #9508, #727, #8798 ) ) ;
#7188 = CARTESIAN_POINT ( 'NONE',  ( 52.34174591811297717, 3.000000000000000000, -12.24483450274845531 ) ) ;
#7189 = EDGE_LOOP ( 'NONE', ( #12279, #9642, #2176, #13282 ) ) ;
#7190 = VERTEX_POINT ( 'NONE', #13579 ) ;
#7191 = CARTESIAN_POINT ( 'NONE',  ( -4.174571361198896824, -1.694065894508600678E-18, 6.065330394303907191 ) ) ;
#7192 = ORIENTED_EDGE ( 'NONE', *, *, #510, .T. ) ;
#7193 = EDGE_CURVE ( 'NONE', #5704, #10071, #11031, .T. ) ;
#7194 = DIRECTION ( 'NONE',  ( -1.000000000000000000, 0.000000000000000000, 0.000000000000000000 ) ) ;
#7195 = CARTESIAN_POINT ( 'NONE',  ( -5.496871281090180972, 0.000000000000000000, 4.899765193453235135 ) ) ;
#7196 = LINE ( 'NONE', #11598, #6216 ) ;
#7197 = CYLINDRICAL_SURFACE ( 'NONE', #10336, 5.500000000000000000 ) ;
#7198 = DIRECTION ( 'NONE',  ( -0.000000000000000000, -1.000000000000000000, -0.000000000000000000 ) ) ;
#7199 = CONTEXT_DEPENDENT_SHAPE_REPRESENTATION ( #12691, #12946 ) ;
#7200 = CARTESIAN_POINT ( 'NONE',  ( 3.000000000000001776, 0.000000000000000000, 7.000000000000000000 ) ) ;
#7201 = EDGE_CURVE ( 'NONE', #2104, #13127, #261, .T. ) ;
#7202 = FACE_OUTER_BOUND ( 'NONE', #12516, .T. ) ;
#7203 = CARTESIAN_POINT ( 'NONE',  ( -5.977417671213807182, 1.734723475976807094E-15, 3.135757960025121527 ) ) ;
#7204 = VERTEX_POINT ( 'NONE', #7578 ) ;
#7205 = CARTESIAN_POINT ( 'NONE',  ( -11.35348746973813761, 3.000000000000000000, -6.343077501554963860 ) ) ;
#7206 = ORIENTED_EDGE ( 'NONE', *, *, #5922, .T. ) ;
#7207 = VERTEX_POINT ( 'NONE', #11710 ) ;
#7208 = ORIENTED_EDGE ( 'NONE', *, *, #864, .F. ) ;
#7209 = EDGE_CURVE ( 'NONE', #13403, #2130, #12692, .T. ) ;
#7210 = EDGE_CURVE ( 'NONE', #12572, #5437, #7950, .T. ) ;
#7211 = ORIENTED_EDGE ( 'NONE', *, *, #2114, .T. ) ;
#7212 = DIRECTION ( 'NONE',  ( 0.000000000000000000, 1.000000000000000000, 0.000000000000000000 ) ) ;
#7213 = CARTESIAN_POINT ( 'NONE',  ( -13.04554897075799680, 3.000000000000000000, -5.733772933379471581 ) ) ;
#7214 = PLANE ( 'NONE',  #254 ) ;
#7215 = FACE_OUTER_BOUND ( 'NONE', #4300, .T. ) ;
#7216 = DIRECTION ( 'NONE',  ( 0.000000000000000000, 1.000000000000000000, -0.000000000000000000 ) ) ;
#7217 = DIRECTION ( 'NONE',  ( -0.8277666712360849388, 0.000000000000000000, -0.5610724890695777400 ) ) ;
#7218 = VERTEX_POINT ( 'NONE', #11645 ) ;
#7219 = CARTESIAN_POINT ( 'NONE',  ( 12.03251085770905959, 0.000000000000000000, 3.999999998926332179 ) ) ;
#7220 = DIRECTION ( 'NONE',  ( 0.000000000000000000, 0.000000000000000000, 1.000000000000000000 ) ) ;
#7221 = EDGE_CURVE ( 'NONE', #11405, #10281, #2200, .T. ) ;
#7222 = ORIENTED_EDGE ( 'NONE', *, *, #4993, .F. ) ;
#7223 = DIRECTION ( 'NONE',  ( -0.000000000000000000, -1.000000000000000000, -0.000000000000000000 ) ) ;
#7224 = APPLICATION_PROTOCOL_DEFINITION ( 'draft international standard', 'automotive_design', 1998, #4404 ) ;
#7225 = CARTESIAN_POINT ( 'NONE',  ( -14.08504230442587790, 0.000000000000000000, -2.161962830978695571 ) ) ;
#7226 = CARTESIAN_POINT ( 'NONE',  ( 2.568302020731520141, 3.000000000000000000, 12.56087513340552420 ) ) ;
#7227 = CARTESIAN_POINT ( 'NONE',  ( -12.38517345876401521, 3.000000000000000000, -12.42191571009144901 ) ) ;
#7228 = B_SPLINE_CURVE_WITH_KNOTS ( 'NONE', 3,
 ( #183, #3326, #11746, #6508 ),
 .UNSPECIFIED., .F., .F.,
 ( 4, 4 ),
 ( 0.1276832474596253097, 1.000000000000000000 ),
 .UNSPECIFIED. ) ;
#7229 = CARTESIAN_POINT ( 'NONE',  ( 12.25836857253663581, 3.000000000000000000, 5.784789447945493990 ) ) ;
#7230 = CARTESIAN_POINT ( 'NONE',  ( -11.52666717836884125, 3.000000000000000000, -3.647470871583627705 ) ) ;
#7231 = APPLICATION_CONTEXT ( 'automotive_design' ) ;
#7232 = ORIENTED_EDGE ( 'NONE', *, *, #6558, .F. ) ;
#7233 = UNCERTAINTY_MEASURE_WITH_UNIT (LENGTH_MEASURE( 1.000000000000000082E-05 ), #12750, 'distance_accuracy_value', 'NONE');
#7234 = EDGE_CURVE ( 'NONE', #11204, #2891, #1286, .T. ) ;
#7235 = VERTEX_POINT ( 'NONE', #4344 ) ;
#7236 = CARTESIAN_POINT ( 'NONE',  ( 0.000000000000000000, 3.000000000000000000, 0.000000000000000000 ) ) ;
#7237 = B_SPLINE_CURVE_WITH_KNOTS ( 'NONE', 2,
 ( #5044, #10496, #11527 ),
 .UNSPECIFIED., .F., .F.,
 ( 3, 3 ),
 ( 0.000000000000000000, 1.000000000000000000 ),
 .UNSPECIFIED. ) ;
#7238 = VERTEX_POINT ( 'NONE', #10684 ) ;
#7239 = SHAPE_REPRESENTATION_RELATIONSHIP ( 'NONE' , 'NONE' ,  #2323, #7847 ) ;
#7240 = DIRECTION ( 'NONE',  ( 0.000000000000000000, 1.000000000000000000, -0.000000000000000000 ) ) ;
#7241 = CARTESIAN_POINT ( 'NONE',  ( 10.18987059060247269, 3.000000000000000000, 6.506507307819714647 ) ) ;
#7242 = CARTESIAN_POINT ( 'NONE',  ( 1.650143266773734796, 3.000000000000000000, -14.90895795148410841 ) ) ;
#7243 = CARTESIAN_POINT ( 'NONE',  ( 52.34174591811297717, 0.000000000000000000, -12.24483450274845531 ) ) ;
#7244 = CARTESIAN_POINT ( 'NONE',  ( 31.00000000000000000, 3.000000000000000000, -4.000000001073670930 ) ) ;
#7245 = ORIENTED_EDGE ( 'NONE', *, *, #12397, .F. ) ;
#7246 = DIRECTION ( 'NONE',  ( -1.000000000000000000, -0.000000000000000000, -0.000000000000000000 ) ) ;
#7247 = ORIENTED_EDGE ( 'NONE', *, *, #3041, .T. ) ;
#7248 = EDGE_CURVE ( 'NONE', #7648, #1815, #11812, .T. ) ;
#7249 = VERTEX_POINT ( 'NONE', #8594 ) ;
#7250 = EDGE_CURVE ( 'NONE', #10192, #710, #5244, .T. ) ;
#7251 = CARTESIAN_POINT ( 'NONE',  ( 6.554160776451332993, 9.000000000000000000, -1.614148852004323675 ) ) ;
#7253 = ORIENTED_EDGE ( 'NONE', *, *, #12986, .F. ) ;
#7252 = B_SPLINE_CURVE_WITH_KNOTS ( 'NONE', 3,
 ( #11491, #13496, #4050, #11571 ),
 .UNSPECIFIED., .F., .F.,
 ( 4, 4 ),
 ( 0.000000000000000000, 0.8452273900860258760 ),
 .UNSPECIFIED. ) ;
#7254 = DIRECTION ( 'NONE',  ( 0.7772490812545771455, 0.000000000000000000, 0.6291930273683233876 ) ) ;
#7255 = FACE_OUTER_BOUND ( 'NONE', #3456, .T. ) ;
#7256 = CARTESIAN_POINT ( 'NONE',  ( 4.164551629694410728, 9.000000000000000000, -6.072874324029720050 ) ) ;
#7257 = CARTESIAN_POINT ( 'NONE',  ( -10.88404822699983576, 3.000000000000000000, 29.60989680561421622 ) ) ;
#7258 = AXIS2_PLACEMENT_3D ( 'NONE', #3090, #7303, #11504 ) ;
#7259 = LINE ( 'NONE', #6093, #7915 ) ;
#7260 = CARTESIAN_POINT ( 'NONE',  ( -14.82803603298502360, 0.000000000000000000, -2.264806262022826644 ) ) ;
#7261 = CARTESIAN_POINT ( 'NONE',  ( 12.00000000000002309, 8.000000000000000000, 10.00000000000000178 ) ) ;
#7262 = CARTESIAN_POINT ( 'NONE',  ( 3.647599401157688437, 3.000000000000000000, 11.52662650599083882 ) ) ;
#7263 = ORIENTED_EDGE ( 'NONE', *, *, #1747, .F. ) ;
#7265 = B_SPLINE_CURVE_WITH_KNOTS ( 'NONE', 3,
 ( #5404, #7278, #9609, #3128 ),
 .UNSPECIFIED., .F., .F.,
 ( 4, 4 ),
 ( 0.000000000000000000, 0.8452273900860258760 ),
 .UNSPECIFIED. ) ;
#7264 = CARTESIAN_POINT ( 'NONE',  ( -7.144272221052618832, 9.000000000000000000, 1.784003156764502940 ) ) ;
#7266 = ADVANCED_FACE ( 'NONE', ( #5435 ), #11780, .T. ) ;
#7267 = ORIENTED_EDGE ( 'NONE', *, *, #4144, .F. ) ;
#7268 = VERTEX_POINT ( 'NONE', #3293 ) ;
#7269 = CIRCLE ( 'NONE', #3320, 3.500000000000000888 ) ;
#7270 = VERTEX_POINT ( 'NONE', #10612 ) ;
#7271 = EDGE_CURVE ( 'NONE', #10338, #9457, #13449, .T. ) ;
#7272 = EDGE_CURVE ( 'NONE', #1406, #4083, #12310, .T. ) ;
#7273 = EDGE_LOOP ( 'NONE', ( #13519, #8442, #6387, #1683 ) ) ;
#7274 = DIRECTION ( 'NONE',  ( 0.000000000000000000, 0.000000000000000000, 1.000000000000000000 ) ) ;
#7275 = CARTESIAN_POINT ( 'NONE',  ( 0.000000000000000000, 3.000000000000000000, 0.000000000000000000 ) ) ;
#7276 = DIRECTION ( 'NONE',  ( -0.000000000000000000, -1.000000000000000000, 0.000000000000000000 ) ) ;
#7277 = AXIS2_PLACEMENT_3D ( 'NONE', #10146, #7938, #3734 ) ;
#7278 = CARTESIAN_POINT ( 'NONE',  ( 8.771102293099069414, 3.000000000000000000, 10.33484986938308303 ) ) ;
#7279 = CARTESIAN_POINT ( 'NONE',  ( -13.03533457366735426, 3.000000000000000000, -6.217402469309218027 ) ) ;
#7280 = VECTOR ( 'NONE', #11599, 1000.000000000000000 ) ;
#7281 = B_SPLINE_CURVE_WITH_KNOTS ( 'NONE', 3,
 ( #12163, #10149, #12813, #11397 ),
 .UNSPECIFIED., .F., .F.,
 ( 4, 4 ),
 ( 0.1276832474596238665, 1.000000000000000000 ),
 .UNSPECIFIED. ) ;
#7282 = B_SPLINE_SURFACE_WITH_KNOTS ( 'NONE', 3, 1, ( 
 ( #2591, #9200 ),
 ( #3832, #13409 ),
 ( #9136, #8033 ),
 ( #1640, #3962 ) ),
 .UNSPECIFIED., .F., .F., .F.,
 ( 4, 4 ),
 ( 2, 2 ),
 ( 0.000000000000000000, 0.5855695330273008592 ),
 ( 0.000000000000000000, 1.000000000000000000 ),
 .UNSPECIFIED. ) ;
#7283 = ORIENTED_EDGE ( 'NONE', *, *, #13300, .T. ) ;
#7284 = DIRECTION ( 'NONE',  ( -0.000000000000000000, -1.000000000000000000, -0.000000000000000000 ) ) ;
#7285 = CARTESIAN_POINT ( 'NONE',  ( 11.46847481510586775, 0.000000000000000000, 5.708888906988908829 ) ) ;
#7286 = VECTOR ( 'NONE', #551, 1000.000000000000000 ) ;
#7287 = ORIENTED_EDGE ( 'NONE', *, *, #4929, .F. ) ;
#7288 = CARTESIAN_POINT ( 'NONE',  ( -7.668956737359326148, 0.000000000000000000, -2.066866683227997825 ) ) ;
#7289 = DIRECTION ( 'NONE',  ( 0.000000000000000000, 0.000000000000000000, -1.000000000000000000 ) ) ;
#7290 = SHAPE_DEFINITION_REPRESENTATION ( #12709, #3798 ) ;
#7291 = CARTESIAN_POINT ( 'NONE',  ( 6.554160776451332993, 9.000000000000000000, -1.614148852004323675 ) ) ;
#7292 = DIRECTION ( 'NONE',  ( 0.000000000000000000, 0.000000000000000000, 1.000000000000000000 ) ) ;
#7293 = CARTESIAN_POINT ( 'NONE',  ( 9.250000000000003553, 2.750000000000000888, 10.00000000000000000 ) ) ;
#7294 = CIRCLE ( 'NONE', #2445, 1.499999999999998668 ) ;
#7295 = AXIS2_PLACEMENT_3D ( 'NONE', #10307, #873, #13196 ) ;
#7296 = DIRECTION ( 'NONE',  ( -0.000000000000000000, -1.000000000000000000, -0.000000000000000000 ) ) ;
#7297 = CYLINDRICAL_SURFACE ( 'NONE', #10204, 3.500000000000000888 ) ;
#7298 = ORIENTED_EDGE ( 'NONE', *, *, #1720, .T. ) ;
#7299 = VERTEX_POINT ( 'NONE', #9773 ) ;
#7300 = CARTESIAN_POINT ( 'NONE',  ( 0.5501230721522984979, 0.000000000000000000, -12.98835496148321766 ) ) ;
#7301 = ORIENTED_EDGE ( 'NONE', *, *, #3694, .T. ) ;
#7302 = CIRCLE ( 'NONE', #3551, 3.499999999999999556 ) ;
#7303 = DIRECTION ( 'NONE',  ( 0.000000000000000000, 1.000000000000000000, 0.000000000000000000 ) ) ;
#7304 = FILL_AREA_STYLE ('',( #9498 ) ) ;
#7305 = CARTESIAN_POINT ( 'NONE',  ( -13.73660796332618261, 0.000000000000000000, -6.025412986832017204 ) ) ;
#7306 = FACE_OUTER_BOUND ( 'NONE', #7714, .T. ) ;
#7307 = LINE ( 'NONE', #8198, #4214 ) ;
#7308 = B_SPLINE_CURVE_WITH_KNOTS ( 'NONE', 3,
 ( #5540, #2444, #4443, #3410 ),
 .UNSPECIFIED., .F., .F.,
 ( 4, 4 ),
 ( 0.000000000000000000, 0.5855695330273008592 ),
 .UNSPECIFIED. ) ;
#7309 = CARTESIAN_POINT ( 'NONE',  ( -4.577511697546077230, 0.000000000000000000, -12.75843939030334795 ) ) ;
#7310 = VERTEX_POINT ( 'NONE', #90 ) ;
#7311 = CARTESIAN_POINT ( 'NONE',  ( -2.481593227817850966, 9.000000000000000000, -8.129679886173169834 ) ) ;
#7312 = AXIS2_PLACEMENT_3D ( 'NONE', #12657, #12273, #7022 ) ;
#7313 = ORIENTED_EDGE ( 'NONE', *, *, #8613, .T. ) ;
#7314 = EDGE_LOOP ( 'NONE', ( #10400, #9403, #2535, #10312 ) ) ;
#7315 = DIRECTION ( 'NONE',  ( 0.000000000000000000, 1.000000000000000000, 0.000000000000000000 ) ) ;
#7316 = ORIENTED_EDGE ( 'NONE', *, *, #1288, .T. ) ;
#7317 = CARTESIAN_POINT ( 'NONE',  ( 0.000000000000000000, 0.000000000000000000, 0.000000000000000000 ) ) ;
#7318 = CIRCLE ( 'NONE', #6881, 1.499999999999998668 ) ;
#7319 = DIRECTION ( 'NONE',  ( -0.000000000000000000, -1.000000000000000000, -0.000000000000000000 ) ) ;
#7320 = VECTOR ( 'NONE', #4285, 1000.000000000000000 ) ;
#7321 = CIRCLE ( 'NONE', #8190, 0.1000000000000000472 ) ;
#7322 = CARTESIAN_POINT ( 'NONE',  ( 12.08646469655232636, 0.000000000000000000, -8.883544964652022813 ) ) ;
#7323 = CARTESIAN_POINT ( 'NONE',  ( 4.690415759823430619, 0.000000000000000000, 4.500000000000000888 ) ) ;
#7324 = EDGE_CURVE ( 'NONE', #13528, #7270, #3170, .T. ) ;
#7325 = CARTESIAN_POINT ( 'NONE',  ( -5.708888906988910605, 0.000000000000000000, 11.46847481510586597 ) ) ;
#7326 = CARTESIAN_POINT ( 'NONE',  ( -7.780961115628988622, 9.000000000000000000, -3.421497350147985728 ) ) ;
#7327 = CARTESIAN_POINT ( 'NONE',  ( -4.174571361198896824, 9.000000000000000000, 6.065330394303907191 ) ) ;
#7328 = CARTESIAN_POINT ( 'NONE',  ( 2.720000000000001528, 2.000000000000000000, 6.000000000000000000 ) ) ;
#7329 = ORIENTED_EDGE ( 'NONE', *, *, #7018, .F. ) ;
#7330 = LINE ( 'NONE', #5200, #9296 ) ;
#7331 = VERTEX_POINT ( 'NONE', #3368 ) ;
#7332 = AXIS2_PLACEMENT_3D ( 'NONE', #7082, #13284, #3842 ) ;
#7333 = VERTEX_POINT ( 'NONE', #2344 ) ;
#7334 = CIRCLE ( 'NONE', #9953, 14.25000000000000178 ) ;
#7335 = CIRCLE ( 'NONE', #1613, 5.500000000000000000 ) ;
#7336 = ORIENTED_EDGE ( 'NONE', *, *, #2231, .F. ) ;
#7337 = ORIENTED_EDGE ( 'NONE', *, *, #13267, .T. ) ;
#7338 = CARTESIAN_POINT ( 'NONE',  ( 2.999999999999995559, 2.000000000000000000, -10.00000000000000355 ) ) ;
#7339 = EDGE_CURVE ( 'NONE', #3503, #7648, #2405, .T. ) ;
#7340 = EDGE_CURVE ( 'NONE', #7331, #8551, #6636, .T. ) ;
#7341 = FACE_OUTER_BOUND ( 'NONE', #2129, .T. ) ;
#7342 = AXIS2_PLACEMENT_3D ( 'NONE', #9791, #11660, #11733 ) ;
#7343 = CARTESIAN_POINT ( 'NONE',  ( -10.18979803820052155, 0.000000000000000000, 6.506620931068709091 ) ) ;
#7344 = DIRECTION ( 'NONE',  ( -0.000000000000000000, -1.000000000000000000, -0.000000000000000000 ) ) ;
#7345 = EDGE_CURVE ( 'NONE', #10414, #12082, #12377, .T. ) ;
#7346 = EDGE_CURVE ( 'NONE', #1668, #5256, #6338, .T. ) ;
#7347 = ORIENTED_EDGE ( 'NONE', *, *, #7418, .T. ) ;
#7348 = VERTEX_POINT ( 'NONE', #8666 ) ;
#7349 = CARTESIAN_POINT ( 'NONE',  ( -10.18987059060247624, 3.000000000000000000, -6.506507307819711095 ) ) ;
#7350 = AXIS2_PLACEMENT_3D ( 'NONE', #8030, #8095, #11471 ) ;
#7351 = CARTESIAN_POINT ( 'NONE',  ( 2.525608486058770641, 3.000000000000000000, 2.423076923076923350 ) ) ;
#7352 = AXIS2_PLACEMENT_3D ( 'NONE', #9772, #7703, #11778 ) ;
#7353 = VERTEX_POINT ( 'NONE', #10805 ) ;
#7354 = CARTESIAN_POINT ( 'NONE',  ( 8.914835885878220623, 0.000000000000000000, -11.11702303352196708 ) ) ;
#7355 = EDGE_CURVE ( 'NONE', #13143, #6903, #9503, .T. ) ;
#7356 = CARTESIAN_POINT ( 'NONE',  ( 2.720000000000001528, 0.000000000000000000, 6.000000000000000000 ) ) ;
#7357 = SHAPE_DEFINITION_REPRESENTATION ( #7775, #8539 ) ;
#7358 = DIRECTION ( 'NONE',  ( -1.000000000000000000, -0.000000000000000000, -0.000000000000000000 ) ) ;
#7359 = CARTESIAN_POINT ( 'NONE',  ( 11.70905276178455878, 0.000000000000000000, -9.375397774054460953 ) ) ;
#7360 = VECTOR ( 'NONE', #1765, 1000.000000000000000 ) ;
#7361 = PLANE ( 'NONE',  #5596 ) ;
#7362 = CIRCLE ( 'NONE', #10879, 2.999999999999999112 ) ;
#7363 = EDGE_CURVE ( 'NONE', #5524, #4532, #4583, .T. ) ;
#7364 = LINE ( 'NONE', #1992, #1886 ) ;
#7365 = VECTOR ( 'NONE', #10755, 1000.000000000000000 ) ;
#7366 = CARTESIAN_POINT ( 'NONE',  ( 0.000000000000000000, 3.000000000000000000, 1.500000000000000000 ) ) ;
#7367 = ORIENTED_EDGE ( 'NONE', *, *, #5007, .F. ) ;
#7368 = ORIENTED_EDGE ( 'NONE', *, *, #7843, .F. ) ;
#7369 = ORIENTED_EDGE ( 'NONE', *, *, #8036, .T. ) ;
#7370 = CARTESIAN_POINT ( 'NONE',  ( 0.000000000000000000, 9.000000000000000000, 0.000000000000000000 ) ) ;
#7371 = ORIENTED_EDGE ( 'NONE', *, *, #2172, .F. ) ;
#7372 =( GEOMETRIC_REPRESENTATION_CONTEXT ( 3 ) GLOBAL_UNCERTAINTY_ASSIGNED_CONTEXT ( ( #3645 ) ) GLOBAL_UNIT_ASSIGNED_CONTEXT ( ( #12139, #7109, #2686 ) ) REPRESENTATION_CONTEXT ( 'NONE', 'WORKASPACE' ) );
#7373 = AXIS2_PLACEMENT_3D ( 'NONE', #3035, #11586, #8393 ) ;
#7374 = ADVANCED_FACE ( 'NONE', ( #4542 ), #7777, .T. ) ;
#7375 = ADVANCED_FACE ( 'NONE', ( #13014 ), #6207, .T. ) ;
#7376 = CARTESIAN_POINT ( 'NONE',  ( 7.500000000000003553, 3.000000000000000000, 13.39999999999999858 ) ) ;
#7377 = SURFACE_STYLE_USAGE ( .BOTH. , #1036 ) ;
#7378 = CARTESIAN_POINT ( 'NONE',  ( -12.75843939030334795, 3.000000000000000000, 4.577511697546079006 ) ) ;
#7379 = LINE ( 'NONE', #9636, #3963 ) ;
#7380 = CARTESIAN_POINT ( 'NONE',  ( -2.264806262022998062, 3.000000000000000000, -14.82803603298499340 ) ) ;
#7381 = CARTESIAN_POINT ( 'NONE',  ( -2.375523406013128724, 9.000000000000000000, 6.318179211409233886 ) ) ;
#7382 = LINE ( 'NONE', #8327, #12871 ) ;
#7383 = ORIENTED_EDGE ( 'NONE', *, *, #5513, .F. ) ;
#7384 = DIRECTION ( 'NONE',  ( 0.000000000000000000, 1.000000000000000000, 0.000000000000000000 ) ) ;
#7385 = ORIENTED_EDGE ( 'NONE', *, *, #6518, .F. ) ;
#7386 = CIRCLE ( 'NONE', #12669, 3.500000000000000888 ) ;
#7387 = ORIENTED_EDGE ( 'NONE', *, *, #6673, .T. ) ;
#7388 = EDGE_LOOP ( 'NONE', ( #4682, #13303, #1792, #5408 ) ) ;
#7389 = LINE ( 'NONE', #9515, #7100 ) ;
#7390 = ORIENTED_EDGE ( 'NONE', *, *, #5005, .T. ) ;
#7391 = CARTESIAN_POINT ( 'NONE',  ( 30.73000000000000043, 0.000000000000000000, -3.999999999999999112 ) ) ;
#7392 = COLOUR_RGB ( '',0.7803921568627451011, 0.7607843137254901578, 0.7411764705882353255 ) ;
#7393 = CARTESIAN_POINT ( 'NONE',  ( 7.500000000000003553, 3.000000000000000000, 13.39999999999999858 ) ) ;
#7394 = DIRECTION ( 'NONE',  ( 0.000000000000000000, 0.000000000000000000, 1.000000000000000000 ) ) ;
#7395 = CARTESIAN_POINT ( 'NONE',  ( -6.749999880766614169, 9.000000000000000000, -0.001268720102703135150 ) ) ;
#7396 = FACE_OUTER_BOUND ( 'NONE', #10719, .T. ) ;
#7397 = LINE ( 'NONE', #11332, #964 ) ;
#7398 = EDGE_CURVE ( 'NONE', #175, #6767, #11265, .T. ) ;
#7399 = LINE ( 'NONE', #2994, #10586 ) ;
#7400 = CARTESIAN_POINT ( 'NONE',  ( 10.18987059060247269, 0.000000000000000000, 6.506507307819714647 ) ) ;
#7401 = B_SPLINE_CURVE_WITH_KNOTS ( 'NONE', 3,
 ( #2422, #7461, #5517, #8484 ),
 .UNSPECIFIED., .F., .F.,
 ( 4, 4 ),
 ( 0.000000000000000000, 0.8452273900860258760 ),
 .UNSPECIFIED. ) ;
#7402 = VERTEX_POINT ( 'NONE', #8792 ) ;
#7403 = CARTESIAN_POINT ( 'NONE',  ( -11.52330688609014686, 3.000000000000000000, -6.017756925049552841 ) ) ;
#7404 = ORIENTED_EDGE ( 'NONE', *, *, #8503, .F. ) ;
#7405 = EDGE_LOOP ( 'NONE', ( #5542, #4585, #2761, #374 ) ) ;
#7406 = EDGE_CURVE ( 'NONE', #11209, #7676, #10946, .T. ) ;
#7407 = ORIENTED_EDGE ( 'NONE', *, *, #9849, .F. ) ;
#7408 = VERTEX_POINT ( 'NONE', #3699 ) ;
#7409 = CARTESIAN_POINT ( 'NONE',  ( -5.571313494980134173, 3.000000000000000000, 10.72979803820131295 ) ) ;
#7410 = LINE ( 'NONE', #6509, #5789 ) ;
#7411 = CARTESIAN_POINT ( 'NONE',  ( 26.30958424017656938, 0.000000000000000000, -1.399999999999999911 ) ) ;
#7412 = DIRECTION ( 'NONE',  ( 0.000000000000000000, 1.000000000000000000, 0.000000000000000000 ) ) ;
#7413 = DIRECTION ( 'NONE',  ( 0.000000000000000000, -1.000000000000000000, 0.000000000000000000 ) ) ;
#7414 = EDGE_LOOP ( 'NONE', ( #1001, #4331, #9440, #11003 ) ) ;
#7415 = VERTEX_POINT ( 'NONE', #620 ) ;
#7416 = EDGE_CURVE ( 'NONE', #5310, #3210, #274, .T. ) ;
#7417 = DIRECTION ( 'NONE',  ( 0.000000000000000000, 0.000000000000000000, -1.000000000000000000 ) ) ;
#7418 = EDGE_CURVE ( 'NONE', #5898, #8692, #7743, .T. ) ;
#7419 = B_SPLINE_SURFACE_WITH_KNOTS ( 'NONE', 3, 1, ( 
 ( #13451, #4200 ),
 ( #8396, #3100 ),
 ( #12625, #3930 ),
 ( #7311, #2081 ) ),
 .UNSPECIFIED., .F., .F., .F.,
 ( 4, 4 ),
 ( 2, 2 ),
 ( 0.000000000000000000, 0.8724294488011762327 ),
 ( 0.000000000000000000, 1.000000000000000000 ),
 .UNSPECIFIED. ) ;
#7420 = EDGE_LOOP ( 'NONE', ( #3436, #10638, #1031, #4029 ) ) ;
#7421 = DIRECTION ( 'NONE',  ( -0.000000000000000000, -1.000000000000000000, -0.000000000000000000 ) ) ;
#7422 = EDGE_CURVE ( 'NONE', #8734, #12207, #3639, .T. ) ;
#7423 = CARTESIAN_POINT ( 'NONE',  ( 0.000000000000000000, 3.000000000000000000, 0.000000000000000000 ) ) ;
#7424 = CARTESIAN_POINT ( 'NONE',  ( 5.170206418547604876, 3.000000000000000000, -13.27898586450069196 ) ) ;
#7425 = CARTESIAN_POINT ( 'NONE',  ( 7.248474140376192310, 9.000000000000000000, 4.439552076088041588 ) ) ;
#7426 = CARTESIAN_POINT ( 'NONE',  ( -8.482622935103766082, 0.000000000000000000, 9.600126836553263487 ) ) ;
#7427 = CARTESIAN_POINT ( 'NONE',  ( 28.54655175640005282, 3.000000000000000000, -2.353846153846155254 ) ) ;
#7428 = AXIS2_PLACEMENT_3D ( 'NONE', #5585, #3582, #6693 ) ;
#7429 = CARTESIAN_POINT ( 'NONE',  ( 3.000000000000001776, 0.000000000000000000, 10.00000000000000000 ) ) ;
#7430 = ADVANCED_FACE ( 'NONE', ( #12947 ), #6742, .T. ) ;
#7431 = ORIENTED_EDGE ( 'NONE', *, *, #9312, .T. ) ;
#7432 = ORIENTED_EDGE ( 'NONE', *, *, #11466, .F. ) ;
#7433 = ORIENTED_EDGE ( 'NONE', *, *, #1059, .T. ) ;
#7434 = CARTESIAN_POINT ( 'NONE',  ( 19.65244806805498001, 3.000000000000000000, -5.000000000000000000 ) ) ;
#7435 = VERTEX_POINT ( 'NONE', #6681 ) ;
#7436 = ADVANCED_FACE ( 'NONE', ( #5775 ), #2606, .T. ) ;
#7437 = ADVANCED_FACE ( 'NONE', ( #4680 ), #6802, .T. ) ;
#7438 = B_SPLINE_SURFACE_WITH_KNOTS ( 'NONE', 3, 1, ( 
 ( #10524, #6251 ),
 ( #1083, #3146 ),
 ( #6315, #2181 ),
 ( #10464, #4324 ) ),
 .UNSPECIFIED., .F., .F., .F.,
 ( 4, 4 ),
 ( 2, 2 ),
 ( 0.000000000000000000, 0.5855695330273008592 ),
 ( 0.000000000000000000, 1.000000000000000000 ),
 .UNSPECIFIED. ) ;
#7439 = DIRECTION ( 'NONE',  ( 0.000000000000000000, 0.000000000000000000, 1.000000000000000000 ) ) ;
#7440 = CARTESIAN_POINT ( 'NONE',  ( 5.733772933379474246, 3.000000000000000000, -13.04554897075799502 ) ) ;
#7441 = DIRECTION ( 'NONE',  ( -0.000000000000000000, -1.000000000000000000, -0.000000000000000000 ) ) ;
#7442 = CARTESIAN_POINT ( 'NONE',  ( -8.883544964652065445, 0.000000000000000000, -12.08646469655229438 ) ) ;
#7443 = CARTESIAN_POINT ( 'NONE',  ( 9.375397774054407662, 0.000000000000000000, -11.70905276178460497 ) ) ;
#7444 = CARTESIAN_POINT ( 'NONE',  ( -10.98198414889942676, 0.000000000000000000, -9.379342464487661957 ) ) ;
#7445 = ORIENTED_EDGE ( 'NONE', *, *, #8943, .T. ) ;
#7446 = CARTESIAN_POINT ( 'NONE',  ( -12.07794044664754018, 3.000000000000000000, -0.5398653231797256868 ) ) ;
#7447 = ORIENTED_EDGE ( 'NONE', *, *, #10821, .F. ) ;
#7448 = EDGE_CURVE ( 'NONE', #6498, #3500, #9510, .T. ) ;
#7449 = ORIENTED_EDGE ( 'NONE', *, *, #11492, .F. ) ;
#7450 = EDGE_CURVE ( 'NONE', #12351, #9536, #4812, .T. ) ;
#7451 = EDGE_LOOP ( 'NONE', ( #7552, #2789, #8657, #932 ) ) ;
#7452 = DIRECTION ( 'NONE',  ( 0.000000000000000000, 1.000000000000000000, 0.000000000000000000 ) ) ;
#7453 = VERTEX_POINT ( 'NONE', #7705 ) ;
#7454 = ADVANCED_FACE ( 'NONE', ( #11915 ), #4444, .F. ) ;
#7455 = CARTESIAN_POINT ( 'NONE',  ( 2.453448243599949397, 0.000000000000000000, -2.353846153846154365 ) ) ;
#7456 =( NAMED_UNIT ( * ) PLANE_ANGLE_UNIT ( ) SI_UNIT ( $, .RADIAN. ) );
#7457 = CARTESIAN_POINT ( 'NONE',  ( -12.60833596047604210, 3.000000000000000000, -3.188441730140805674 ) ) ;
#7458 = CARTESIAN_POINT ( 'NONE',  ( -10.72979803820123479, 3.000000000000000000, -5.571313494980285164 ) ) ;
#7459 = CARTESIAN_POINT ( 'NONE',  ( -12.76342233970728124, 3.000000000000000000, -4.564691384634500970 ) ) ;
#7460 = DIRECTION ( 'NONE',  ( 0.000000000000000000, -1.000000000000000000, 0.000000000000000000 ) ) ;
#7461 = CARTESIAN_POINT ( 'NONE',  ( -12.25282671965375236, 0.000000000000000000, 5.797378255456025364 ) ) ;
#7462 = CARTESIAN_POINT ( 'NONE',  ( -9.324917476840782982, 3.000000000000000000, -9.065441278446241924 ) ) ;
#7463 = EDGE_LOOP ( 'NONE', ( #6211, #4407, #6224, #11902 ) ) ;
#7464 = CARTESIAN_POINT ( 'NONE',  ( -11.52662650599092409, 0.000000000000000000, 3.647599401157420651 ) ) ;
#7465 = ADVANCED_FACE ( 'NONE', ( #10259 ), #11606, .F. ) ;
#7466 = ORIENTED_EDGE ( 'NONE', *, *, #12219, .F. ) ;
#7467 = EDGE_CURVE ( 'NONE', #3538, #9896, #11488, .T. ) ;
#7468 = EDGE_LOOP ( 'NONE', ( #2427, #5678 ) ) ;
#7469 = ORIENTED_EDGE ( 'NONE', *, *, #7896, .T. ) ;
#7470 = AXIS2_PLACEMENT_3D ( 'NONE', #4806, #1718, #137 ) ;
#7471 = CARTESIAN_POINT ( 'NONE',  ( 0.000000000000000000, 9.000000000000000000, 0.000000000000000000 ) ) ;
#7472 = DIRECTION ( 'NONE',  ( -0.000000000000000000, -1.000000000000000000, -0.000000000000000000 ) ) ;
#7473 = DIRECTION ( 'NONE',  ( 0.000000000000000000, 1.000000000000000000, 0.000000000000000000 ) ) ;
#7474 = CARTESIAN_POINT ( 'NONE',  ( -11.13895890373326836, 0.000000000000000000, 7.723663868796768028 ) ) ;
#7475 = CARTESIAN_POINT ( 'NONE',  ( 0.000000000000000000, 3.000000000000000000, 0.000000000000000000 ) ) ;
#7476 = CARTESIAN_POINT ( 'NONE',  ( -4.056222772158361245, 0.000000000000000000, 12.16218796965919324 ) ) ;
#7477 = ORIENTED_EDGE ( 'NONE', *, *, #12349, .T. ) ;
#7478 = ORIENTED_EDGE ( 'NONE', *, *, #3581, .F. ) ;
#7479 = CYLINDRICAL_SURFACE ( 'NONE', #66, 1.000000000000000888 ) ;
#7480 = ORIENTED_EDGE ( 'NONE', *, *, #49, .F. ) ;
#7481 = LINE ( 'NONE', #11686, #5566 ) ;
#7482 = AXIS2_PLACEMENT_3D ( 'NONE', #4987, #1826, #5195 ) ;
#7483 =( REPRESENTATION_RELATIONSHIP ('NONE','NONE', #3798, #8539 ) REPRESENTATION_RELATIONSHIP_WITH_TRANSFORMATION ( #12027 )SHAPE_REPRESENTATION_RELATIONSHIP( ) );
#7484 = COLOUR_RGB ( '',0.7921568627450980005, 0.8196078431372548767, 0.9333333333333333481 ) ;
#7485 = CARTESIAN_POINT ( 'NONE',  ( 0.000000000000000000, 3.000000000000000000, 0.000000000000000000 ) ) ;
#7486 = DIRECTION ( 'NONE',  ( -0.000000000000000000, -1.000000000000000000, -0.000000000000000000 ) ) ;
#7487 = CARTESIAN_POINT ( 'NONE',  ( 2.568302020731520141, 0.000000000000000000, 12.56087513340552420 ) ) ;
#7488 = EDGE_CURVE ( 'NONE', #9824, #4801, #3562, .T. ) ;
#7489 = CARTESIAN_POINT ( 'NONE',  ( -13.86115248177182835, 3.000000000000000000, -5.741477348071267528 ) ) ;
#7490 = CARTESIAN_POINT ( 'NONE',  ( 0.000000000000000000, 3.000000000000000000, -1.500000000000000222 ) ) ;
#7491 = CARTESIAN_POINT ( 'NONE',  ( 0.5398653231797245766, 0.000000000000000000, -12.07794044664754018 ) ) ;
#7492 = ORIENTED_EDGE ( 'NONE', *, *, #13582, .F. ) ;
#7493 = VECTOR ( 'NONE', #199, 1000.000000000000000 ) ;
#7494 = ORIENTED_EDGE ( 'NONE', *, *, #9108, .F. ) ;
#7495 = ORIENTED_EDGE ( 'NONE', *, *, #10386, .T. ) ;
#7496 = CARTESIAN_POINT ( 'NONE',  ( -8.914835885878215294, 3.000000000000000000, 11.11702303352197063 ) ) ;
#7497 = ORIENTED_EDGE ( 'NONE', *, *, #4220, .F. ) ;
#7498 = CARTESIAN_POINT ( 'NONE',  ( 0.000000000000000000, 0.000000000000000000, 0.000000000000000000 ) ) ;
#7499 = PRESENTATION_STYLE_ASSIGNMENT (( #8322 ) ) ;
#7500 = CIRCLE ( 'NONE', #2660, 1.499999999999998668 ) ;
#7501 = EDGE_CURVE ( 'NONE', #6311, #1501, #128, .T. ) ;
#7502 = CARTESIAN_POINT ( 'NONE',  ( 0.000000000000000000, -3.000000000000000000, 0.000000000000000000 ) ) ;
#7503 = CIRCLE ( 'NONE', #11437, 3.500000000000000888 ) ;
#7504 = EDGE_CURVE ( 'NONE', #3318, #10776, #12413, .T. ) ;
#7505 = DIRECTION ( 'NONE',  ( 0.000000000000000000, 0.000000000000000000, 1.000000000000000000 ) ) ;
#7506 = CYLINDRICAL_SURFACE ( 'NONE', #7696, 1.500000000000000666 ) ;
#7507 = CARTESIAN_POINT ( 'NONE',  ( -4.056222772158361245, 3.000000000000000000, 12.16218796965919324 ) ) ;
#7508 = FACE_OUTER_BOUND ( 'NONE', #8677, .T. ) ;
#7509 = ORIENTED_EDGE ( 'NONE', *, *, #12490, .F. ) ;
#7510 = EDGE_CURVE ( 'NONE', #10535, #7268, #826, .T. ) ;
#7511 = CARTESIAN_POINT ( 'NONE',  ( 7.363612555047485131, 9.000000000000000000, -0.02242701489043354146 ) ) ;
#7512 = ORIENTED_EDGE ( 'NONE', *, *, #2615, .F. ) ;
#7513 = EDGE_CURVE ( 'NONE', #2693, #8207, #1862, .T. ) ;
#7514 = EDGE_LOOP ( 'NONE', ( #5275, #2559, #5986, #12081 ) ) ;
#7515 = VERTEX_POINT ( 'NONE', #11679 ) ;
#7516 = CARTESIAN_POINT ( 'NONE',  ( 47.14458624375820506, 3.000000000000000000, -3.829406728833672613 ) ) ;
#7517 = VECTOR ( 'NONE', #7135, 1000.000000000000227 ) ;
#7518 = ORIENTED_EDGE ( 'NONE', *, *, #3970, .F. ) ;
#7519 = CARTESIAN_POINT ( 'NONE',  ( -12.07794044664754018, 3.000000000000000000, -0.5398653231797256868 ) ) ;
#7520 = LINE ( 'NONE', #4284, #4950 ) ;
#7521 = LINE ( 'NONE', #5314, #3131 ) ;
#7522 = EDGE_CURVE ( 'NONE', #12066, #11648, #6061, .T. ) ;
#7523 = DIRECTION ( 'NONE',  ( -0.000000000000000000, -1.000000000000000000, -0.000000000000000000 ) ) ;
#7524 = CARTESIAN_POINT ( 'NONE',  ( 0.000000000000000000, 3.000000000000000000, 0.000000000000000000 ) ) ;
#7525 = AXIS2_PLACEMENT_3D ( 'NONE', #2240, #7551, #3211 ) ;
#7526 = AXIS2_PLACEMENT_3D ( 'NONE', #1511, #3772, #1724 ) ;
#7527 = LINE ( 'NONE', #11735, #13464 ) ;
#7528 = LINE ( 'NONE', #5658, #3615 ) ;
#7529 = ORIENTED_EDGE ( 'NONE', *, *, #8008, .F. ) ;
#7530 = CARTESIAN_POINT ( 'NONE',  ( -12.14623037080100865, 0.000000000000000000, 4.072642252455982437 ) ) ;
#7531 = PRODUCT ( 'gear-link-2', 'gear-link-2', '', ( #10770 ) ) ;
#7532 = EDGE_CURVE ( 'NONE', #7218, #12590, #2468, .T. ) ;
#7533 = VERTEX_POINT ( 'NONE', #685 ) ;
#7534 = ORIENTED_EDGE ( 'NONE', *, *, #9266, .F. ) ;
#7535 = ORIENTED_EDGE ( 'NONE', *, *, #10402, .T. ) ;
#7536 = AXIS2_PLACEMENT_3D ( 'NONE', #8600, #7713, #5442 ) ;
#7537 = AXIS2_PLACEMENT_3D ( 'NONE', #10249, #945, #745 ) ;
#7538 = CIRCLE ( 'NONE', #8623, 3.000000000000000000 ) ;
#7539 = FACE_OUTER_BOUND ( 'NONE', #3397, .T. ) ;
#7540 = CYLINDRICAL_SURFACE ( 'NONE', #11555, 1.500000000000003997 ) ;
#7541 = EDGE_CURVE ( 'NONE', #10341, #1734, #3744, .T. ) ;
#7542 = CARTESIAN_POINT ( 'NONE',  ( 10.18987059060247269, 0.000000000000000000, 6.506507307819714647 ) ) ;
#7543 = CARTESIAN_POINT ( 'NONE',  ( 7.702138240596516638, 3.000000000000000000, -27.99999999999999289 ) ) ;
#7544 = DIRECTION ( 'NONE',  ( 0.000000000000000000, 1.000000000000000000, 0.000000000000000000 ) ) ;
#7545 = AXIS2_PLACEMENT_3D ( 'NONE', #9274, #10456, #1018 ) ;
#7546 = CARTESIAN_POINT ( 'NONE',  ( 0.000000000000000000, 9.000000000000000000, 0.000000000000000000 ) ) ;
#7547 = VECTOR ( 'NONE', #3830, 1000.000000000000000 ) ;
#7548 = CIRCLE ( 'NONE', #3805, 12.08999999999737440 ) ;
#7549 = EDGE_LOOP ( 'NONE', ( #9086, #7024 ) ) ;
#7550 = ORIENTED_EDGE ( 'NONE', *, *, #1183, .F. ) ;
#7551 = DIRECTION ( 'NONE',  ( 0.000000000000000000, 1.000000000000000000, -0.000000000000000000 ) ) ;
#7552 = ORIENTED_EDGE ( 'NONE', *, *, #7177, .T. ) ;
#7553 = CARTESIAN_POINT ( 'NONE',  ( -14.90895795148411374, 3.000000000000000000, -1.650143266773683726 ) ) ;
#7554 = CIRCLE ( 'NONE', #7562, 2.500000000000000000 ) ;
#7555 = TOROIDAL_SURFACE ( 'NONE', #4924, 1.600000000000004086, 0.1000000000000000056 ) ;
#7556 = AXIS2_PLACEMENT_3D ( 'NONE', #2865, #7217, #9060 ) ;
#7557 = FACE_OUTER_BOUND ( 'NONE', #7388, .T. ) ;
#7558 = DIRECTION ( 'NONE',  ( -0.000000000000000000, -1.000000000000000000, -0.000000000000000000 ) ) ;
#7559 = CARTESIAN_POINT ( 'NONE',  ( -11.52666717836884125, 0.000000000000000000, -3.647470871583627705 ) ) ;
#7560 = LINE ( 'NONE', #2124, #12650 ) ;
#7561 = DIRECTION ( 'NONE',  ( 0.000000000000000000, 0.000000000000000000, 1.000000000000000000 ) ) ;
#7562 = AXIS2_PLACEMENT_3D ( 'NONE', #10303, #10509, #8295 ) ;
#7563 = CARTESIAN_POINT ( 'NONE',  ( 0.000000000000000000, 3.000000000000000000, 0.000000000000000000 ) ) ;
#7564 = AXIS2_PLACEMENT_3D ( 'NONE', #6132, #5100, #7112 ) ;
#7565 = ORIENTED_EDGE ( 'NONE', *, *, #7752, .T. ) ;
#7566 = ORIENTED_EDGE ( 'NONE', *, *, #7272, .F. ) ;
#7567 = ORIENTED_EDGE ( 'NONE', *, *, #2961, .T. ) ;
#7568 = LINE ( 'NONE', #2464, #11283 ) ;
#7569 = ADVANCED_FACE ( 'NONE', ( #5984 ), #2471, .F. ) ;
#7570 = ORIENTED_EDGE ( 'NONE', *, *, #7522, .F. ) ;
#7571 = PLANE ( 'NONE',  #3082 ) ;
#7572 = AXIS2_PLACEMENT_3D ( 'NONE', #5681, #5750, #2649 ) ;
#7573 = SURFACE_STYLE_USAGE ( .BOTH. , #1239 ) ;
#7574 = VECTOR ( 'NONE', #3623, 1000.000000000000000 ) ;
#7575 = LINE ( 'NONE', #8524, #4186 ) ;
#7576 = CARTESIAN_POINT ( 'NONE',  ( 17.00000000000000711, 3.000000000000000000, 12.57924256039205524 ) ) ;
#7577 = CARTESIAN_POINT ( 'NONE',  ( 22.00000000000000000, 3.000000000000000000, 0.000000000000000000 ) ) ;
#7578 = CARTESIAN_POINT ( 'NONE',  ( -13.49999999999999645, 3.000000000000000000, -8.549999999999998934 ) ) ;
#7579 = CARTESIAN_POINT ( 'NONE',  ( 0.000000000000000000, 3.000000000000000000, 0.000000000000000000 ) ) ;
#7580 = VERTEX_POINT ( 'NONE', #6369 ) ;
#7581 = LINE ( 'NONE', #3297, #9304 ) ;
#7582 = ORIENTED_EDGE ( 'NONE', *, *, #5309, .F. ) ;
#7583 = ORIENTED_EDGE ( 'NONE', *, *, #2892, .F. ) ;
#7584 =( GEOMETRIC_REPRESENTATION_CONTEXT ( 3 ) GLOBAL_UNCERTAINTY_ASSIGNED_CONTEXT ( ( #3777 ) ) GLOBAL_UNIT_ASSIGNED_CONTEXT ( ( #12389, #9340, #9133 ) ) REPRESENTATION_CONTEXT ( 'NONE', 'WORKASPACE' ) );
#7585 = VERTEX_POINT ( 'NONE', #6443 ) ;
#7586 = AXIS2_PLACEMENT_3D ( 'NONE', #636, #4830, #7999 ) ;
#7587 = DIRECTION ( 'NONE',  ( -0.000000000000000000, -1.000000000000000000, -0.000000000000000000 ) ) ;
#7588 = EDGE_CURVE ( 'NONE', #1714, #375, #5539, .T. ) ;
#7589 = EDGE_CURVE ( 'NONE', #6099, #11515, #13252, .T. ) ;
#7590 = ORIENTED_EDGE ( 'NONE', *, *, #9416, .T. ) ;
#7591 = CARTESIAN_POINT ( 'NONE',  ( 8.795158114916441505, 3.000000000000000000, -9.573149624528689117 ) ) ;
#7592 = EDGE_CURVE ( 'NONE', #11130, #7605, #13023, .T. ) ;
#7593 = ADVANCED_FACE ( 'NONE', ( #10184 ), #762, .T. ) ;
#7595 = CARTESIAN_POINT ( 'NONE',  ( 0.000000000000000000, 2.900000000000000355, 1.600000000000000311 ) ) ;
#7594 = B_SPLINE_CURVE_WITH_KNOTS ( 'NONE', 3,
 ( #9529, #4294, #7462, #2222 ),
 .UNSPECIFIED., .F., .F.,
 ( 4, 4 ),
 ( 0.3636321741318673806, 0.3930502511895355711 ),
 .UNSPECIFIED. ) ;
#7596 = CARTESIAN_POINT ( 'NONE',  ( 7.500000000000003553, 3.000000000000000000, 13.39999999999999858 ) ) ;
#7597 = CARTESIAN_POINT ( 'NONE',  ( -2.161962830978702677, 0.000000000000000000, 14.08504230442587435 ) ) ;
#7598 =( GEOMETRIC_REPRESENTATION_CONTEXT ( 3 ) GLOBAL_UNCERTAINTY_ASSIGNED_CONTEXT ( ( #6962 ) ) GLOBAL_UNIT_ASSIGNED_CONTEXT ( ( #2357, #8883, #3446 ) ) REPRESENTATION_CONTEXT ( 'NONE', 'WORKASPACE' ) );
#7599 = CARTESIAN_POINT ( 'NONE',  ( 2.604399508763947768, 0.000000000000000000, -11.80615107470197778 ) ) ;
#7600 = VECTOR ( 'NONE', #4477, 1000.000000000000000 ) ;
#7601 = LINE ( 'NONE', #8612, #58 ) ;
#7602 = CARTESIAN_POINT ( 'NONE',  ( 2.720000000000001528, 2.000000000000000000, 6.000000000000000000 ) ) ;
#7603 = ORIENTED_EDGE ( 'NONE', *, *, #9036, .T. ) ;
#7604 = CARTESIAN_POINT ( 'NONE',  ( 2.161962830978677363, 0.000000000000000000, 14.08504230442587613 ) ) ;
#7605 = VERTEX_POINT ( 'NONE', #4577 ) ;
#7606 = VERTEX_POINT ( 'NONE', #8561 ) ;
#7607 = ADVANCED_FACE ( 'NONE', ( #10849 ), #1275, .T. ) ;
#7608 = VERTEX_POINT ( 'NONE', #9671 ) ;
#7609 = DIRECTION ( 'NONE',  ( 0.000000000000000000, 0.000000000000000000, 1.000000000000000000 ) ) ;
#7610 = DIRECTION ( 'NONE',  ( -0.000000000000000000, -1.000000000000000000, -0.000000000000000000 ) ) ;
#7611 = EDGE_CURVE ( 'NONE', #4686, #7453, #6056, .T. ) ;
#7612 = CARTESIAN_POINT ( 'NONE',  ( -2.126404030784648569, 32.33135765298362685, 9.278967525481624179 ) ) ;
#7613 = CARTESIAN_POINT ( 'NONE',  ( 0.6724118135762067183, 0.000000000000000000, -13.82336506795094344 ) ) ;
#7614 = DIRECTION ( 'NONE',  ( 0.000000000000000000, 0.000000000000000000, -1.000000000000000000 ) ) ;
#7615 = DIRECTION ( 'NONE',  ( 0.000000000000000000, 1.000000000000000000, 0.000000000000000000 ) ) ;
#7616 = DIRECTION ( 'NONE',  ( 0.000000000000000000, 1.000000000000000000, -0.000000000000000000 ) ) ;
#7617 = DIRECTION ( 'NONE',  ( 0.000000000000000000, 0.000000000000000000, 1.000000000000000000 ) ) ;
#7618 = ORIENTED_EDGE ( 'NONE', *, *, #12533, .F. ) ;
#7619 = ORIENTED_EDGE ( 'NONE', *, *, #6952, .F. ) ;
#7620 = CARTESIAN_POINT ( 'NONE',  ( 11.11702303352196708, 0.000000000000000000, 8.914835885878218846 ) ) ;
#7621 = EDGE_CURVE ( 'NONE', #2502, #11941, #2441, .T. ) ;
#7622 = EDGE_LOOP ( 'NONE', ( #9780, #8896, #11358, #4579 ) ) ;
#7623 = LINE ( 'NONE', #1223, #11522 ) ;
#7624 = CARTESIAN_POINT ( 'NONE',  ( -13.49999999999999645, 3.000000000000000000, -7.049999999999998934 ) ) ;
#7625 = DIRECTION ( 'NONE',  ( 0.000000000000000000, 1.000000000000000000, 0.000000000000000000 ) ) ;
#7626 = CARTESIAN_POINT ( 'NONE',  ( 3.818534268238711338, 0.000000000000000000, -5.566084444408533116 ) ) ;
#7627 = CARTESIAN_POINT ( 'NONE',  ( -13.04554897075795949, 3.000000000000000000, 5.733772933379550629 ) ) ;
#7628 = B_SPLINE_SURFACE_WITH_KNOTS ( 'NONE', 3, 1, ( 
 ( #6316, #12671 ),
 ( #3147, #5353 ),
 ( #959, #3270 ),
 ( #140, #146 ) ),
 .UNSPECIFIED., .F., .F., .F.,
 ( 4, 4 ),
 ( 2, 2 ),
 ( 0.2280192144657617603, 0.8452273900860258760 ),
 ( 0.000000000000000000, 1.000000000000000000 ),
 .UNSPECIFIED. ) ;
#7629 = DIRECTION ( 'NONE',  ( 0.000000000000000000, 0.000000000000000000, -1.000000000000000000 ) ) ;
#7630 = LINE ( 'NONE', #4387, #13330 ) ;
#7631 = CARTESIAN_POINT ( 'NONE',  ( 3.893011711613070691, 0.000000000000000000, -12.40340517008307231 ) ) ;
#7632 = ORIENTED_EDGE ( 'NONE', *, *, #6041, .F. ) ;
#7633 = ORIENTED_EDGE ( 'NONE', *, *, #6745, .F. ) ;
#7634 = EDGE_CURVE ( 'NONE', #9031, #6069, #1590, .T. ) ;
#7635 = ORIENTED_EDGE ( 'NONE', *, *, #609, .F. ) ;
#7636 = ORIENTED_EDGE ( 'NONE', *, *, #10798, .T. ) ;
#7637 = CARTESIAN_POINT ( 'NONE',  ( 1.119409668803368119, 0.000000000000000000, 13.50845331674225847 ) ) ;
#7638 = VERTEX_POINT ( 'NONE', #11954 ) ;
#7639 = CARTESIAN_POINT ( 'NONE',  ( -5.741477348071430065, 0.000000000000000000, -13.86115248177175374 ) ) ;
#7640 = B_SPLINE_SURFACE_WITH_KNOTS ( 'NONE', 3, 1, ( 
 ( #11694, #6590 ),
 ( #2332, #4256 ),
 ( #1357, #9758 ),
 ( #74, #4388 ) ),
 .UNSPECIFIED., .F., .F., .F.,
 ( 4, 4 ),
 ( 2, 2 ),
 ( 0.1547128134717859205, 1.000000000000000000 ),
 ( 0.000000000000000000, 1.000000000000000000 ),
 .UNSPECIFIED. ) ;
#7641 = DIRECTION ( 'NONE',  ( 0.000000000000000000, 1.000000000000000000, -0.000000000000000000 ) ) ;
#7642 = DIRECTION ( 'NONE',  ( 0.000000000000000000, 0.000000000000000000, 1.000000000000000000 ) ) ;
#7643 = DIRECTION ( 'NONE',  ( 0.000000000000000000, 0.000000000000000000, 1.000000000000000000 ) ) ;
#7644 = CARTESIAN_POINT ( 'NONE',  ( 12.08646469655232636, 0.000000000000000000, -8.883544964652022813 ) ) ;
#7645 = ORIENTED_EDGE ( 'NONE', *, *, #7488, .F. ) ;
#7646 = DIRECTION ( 'NONE',  ( 0.000000000000000000, 0.000000000000000000, -1.000000000000000000 ) ) ;
#7647 = ORIENTED_EDGE ( 'NONE', *, *, #4100, .F. ) ;
#7648 = VERTEX_POINT ( 'NONE', #3535 ) ;
#7649 = ORIENTED_EDGE ( 'NONE', *, *, #6154, .T. ) ;
#7650 = CARTESIAN_POINT ( 'NONE',  ( 45.22938609343211880, 3.000000000000000000, -15.43472716196784233 ) ) ;
#7651 = EDGE_LOOP ( 'NONE', ( #2132, #6466, #6126, #10555 ) ) ;
#7652 = ORIENTED_EDGE ( 'NONE', *, *, #842, .F. ) ;
#7653 = B_SPLINE_CURVE_WITH_KNOTS ( 'NONE', 3,
 ( #11221, #829, #3022, #7230 ),
 .UNSPECIFIED., .F., .F.,
 ( 4, 4 ),
 ( 0.000000000000000000, 0.8452273900860258760 ),
 .UNSPECIFIED. ) ;
#7654 = CARTESIAN_POINT ( 'NONE',  ( -13.03533457366735426, 0.000000000000000000, -6.217402469309218027 ) ) ;
#7655 = CARTESIAN_POINT ( 'NONE',  ( 41.29994854050690378, 3.000000000000000000, -5.141175130212632283 ) ) ;
#7656 = PLANE ( 'NONE',  #5057 ) ;
#7657 = CARTESIAN_POINT ( 'NONE',  ( 0.000000000000000000, 9.000000000000000000, 0.000000000000000000 ) ) ;
#7658 = DIRECTION ( 'NONE',  ( -0.000000000000000000, -1.000000000000000000, -0.000000000000000000 ) ) ;
#7659 = CARTESIAN_POINT ( 'NONE',  ( -13.82336506795071607, 0.000000000000000000, 0.6724118135763649251 ) ) ;
#7660 = EDGE_CURVE ( 'NONE', #5111, #9128, #8191, .T. ) ;
#7661 = ORIENTED_EDGE ( 'NONE', *, *, #10798, .F. ) ;
#7662 = PLANE ( 'NONE',  #12172 ) ;
#7663 = ORIENTED_EDGE ( 'NONE', *, *, #10526, .F. ) ;
#7664 = ORIENTED_EDGE ( 'NONE', *, *, #11017, .F. ) ;
#7665 =( REPRESENTATION_RELATIONSHIP ('NONE','NONE', #3798, #7939 ) REPRESENTATION_RELATIONSHIP_WITH_TRANSFORMATION ( #8824 )SHAPE_REPRESENTATION_RELATIONSHIP( ) );
#7666 = ORIENTED_EDGE ( 'NONE', *, *, #4327, .T. ) ;
#7667 = CARTESIAN_POINT ( 'NONE',  ( 7.151505841916629080, 0.000000000000000000, 1.752496229622501511 ) ) ;
#7668 = CARTESIAN_POINT ( 'NONE',  ( 4.564691384634508964, 0.000000000000000000, -12.76342233970727413 ) ) ;
#7669 = ITEM_DEFINED_TRANSFORMATION ( 'NONE', 'NONE', #11359,  #10007 ) ;
#7670 = CARTESIAN_POINT ( 'NONE',  ( 28.47439151394123158, 0.09999999999999982514, -2.423076923076924682 ) ) ;
#7671 = EDGE_CURVE ( 'NONE', #11851, #7415, #4228, .T. ) ;
#7672 = CARTESIAN_POINT ( 'NONE',  ( 1.132798289211301698E-15, -3.000000000000000000, -9.250000000000000000 ) ) ;
#7673 = DIRECTION ( 'NONE',  ( 1.000000000000000000, -0.000000000000000000, -9.145772869372436484E-17 ) ) ;
#7674 = DIRECTION ( 'NONE',  ( -0.000000000000000000, -1.000000000000000000, -0.000000000000000000 ) ) ;
#7675 = EDGE_CURVE ( 'NONE', #2426, #3437, #4559, .T. ) ;
#7676 = VERTEX_POINT ( 'NONE', #4439 ) ;
#7677 = EDGE_CURVE ( 'NONE', #8335, #11680, #299, .T. ) ;
#7678 = ORIENTED_EDGE ( 'NONE', *, *, #9257, .T. ) ;
#7679 = ADVANCED_FACE ( 'NONE', ( #10774 ), #8828, .T. ) ;
#7680 = DIRECTION ( 'NONE',  ( 1.000000000000000000, 0.000000000000000000, 1.224646799147353207E-16 ) ) ;
#7681 = ORIENTED_EDGE ( 'NONE', *, *, #720, .T. ) ;
#7682 = CARTESIAN_POINT ( 'NONE',  ( 8.180229652970799847, 3.000000000000000000, -11.90209577080762848 ) ) ;
#7683 = DIRECTION ( 'NONE',  ( 0.000000000000000000, 0.000000000000000000, 1.000000000000000000 ) ) ;
#7684 = CYLINDRICAL_SURFACE ( 'NONE', #79, 14.25000000000000178 ) ;
#7685 = DIRECTION ( 'NONE',  ( -0.000000000000000000, -1.000000000000000000, -0.000000000000000000 ) ) ;
#7686 = DIRECTION ( 'NONE',  ( 0.000000000000000000, 0.000000000000000000, -1.000000000000000000 ) ) ;
#7687 = CIRCLE ( 'NONE', #10102, 8.500000000000000000 ) ;
#7688 = CARTESIAN_POINT ( 'NONE',  ( 5.985774866078161338, 9.000000000000000000, 3.119775513178307147 ) ) ;
#7689 = DIRECTION ( 'NONE',  ( 0.000000000000000000, 0.000000000000000000, 1.000000000000000000 ) ) ;
#7690 = CARTESIAN_POINT ( 'NONE',  ( -5.170206418547117266, 0.000000000000000000, 13.27898586450088203 ) ) ;
#7691 = ORIENTED_EDGE ( 'NONE', *, *, #5983, .T. ) ;
#7692 = ORIENTED_EDGE ( 'NONE', *, *, #8008, .T. ) ;
#7693 = ORIENTED_EDGE ( 'NONE', *, *, #11163, .F. ) ;
#7694 = EDGE_LOOP ( 'NONE', ( #10753, #2675, #3517, #8488, #9063, #9713, #4101, #13191, #3175, #3954, #3841, #12956, #11787, #12647, #6231, #1205, #4702, #13522, #8815, #3285, #11619, #2017, #282, #1604, #11591, #12422, #6975, #5094, #10457, #6850, #11554, #4628, #4319, #12523, #5990, #188, #11795, #339, #8719, #12486, #12969, #5822, #13525, #2480, #9981, #4944, #12076, #5289, #11856, #4836, #12016, #2608, #765 ) ) ;
#7695 = CARTESIAN_POINT ( 'NONE',  ( 0.7901945867173618687, 0.000000000000000000, 12.78643498603817541 ) ) ;
#7696 = AXIS2_PLACEMENT_3D ( 'NONE', #7577, #5120, #11779 ) ;
#7697 = AXIS2_PLACEMENT_3D ( 'NONE', #7596, #1320, #8606 ) ;
#7698 = VERTEX_POINT ( 'NONE', #1417 ) ;
#7699 = DIRECTION ( 'NONE',  ( -0.000000000000000000, -1.000000000000000000, -0.000000000000000000 ) ) ;
#7700 = ADVANCED_FACE ( 'NONE', ( #4644 ), #5534, .F. ) ;
#7701 = CARTESIAN_POINT ( 'NONE',  ( 0.000000000000000000, 3.000000000000000000, 0.000000000000000000 ) ) ;
#7702 = EDGE_CURVE ( 'NONE', #11016, #4379, #9930, .T. ) ;
#7703 = DIRECTION ( 'NONE',  ( 0.000000000000000000, 1.000000000000000000, -0.000000000000000000 ) ) ;
#7704 = AXIS2_PLACEMENT_3D ( 'NONE', #11424, #4251, #8447 ) ;
#7705 = CARTESIAN_POINT ( 'NONE',  ( 0.4639228963249704130, 0.000000000000000000, 8.487330295579726069 ) ) ;
#7706 = AXIS2_PLACEMENT_3D ( 'NONE', #4894, #13443, #3925 ) ;
#7707 = FACE_OUTER_BOUND ( 'NONE', #6531, .T. ) ;
#7708 = VERTEX_POINT ( 'NONE', #187 ) ;
#7709 = CARTESIAN_POINT ( 'NONE',  ( 8.481367827640703183, 9.000000000000000000, 0.5624942419805127880 ) ) ;
#7710 = EDGE_CURVE ( 'NONE', #7190, #5839, #934, .T. ) ;
#7711 = EDGE_LOOP ( 'NONE', ( #1697, #7582 ) ) ;
#7712 = ORIENTED_EDGE ( 'NONE', *, *, #6394, .T. ) ;
#7713 = DIRECTION ( 'NONE',  ( -0.000000000000000000, -1.000000000000000000, -0.000000000000000000 ) ) ;
#7714 = EDGE_LOOP ( 'NONE', ( #11266, #7026, #1109, #1420 ) ) ;
#7715 = AXIS2_PLACEMENT_3D ( 'NONE', #6713, #4371, #441 ) ;
#7716 = EDGE_LOOP ( 'NONE', ( #13247, #9383, #9856, #7764 ) ) ;
#7717 = AXIS2_PLACEMENT_3D ( 'NONE', #472, #10045, #6738 ) ;
#7718 = CARTESIAN_POINT ( 'NONE',  ( -13.82336506795094522, 3.000000000000000000, -0.6724118135761603110 ) ) ;
#7719 = PRESENTATION_STYLE_ASSIGNMENT (( #12005 ) ) ;
#7720 = CARTESIAN_POINT ( 'NONE',  ( -14.82803603298502360, 3.000000000000000000, -2.264806262022826644 ) ) ;
#7721 = FACE_OUTER_BOUND ( 'NONE', #1360, .T. ) ;
#7722 = CARTESIAN_POINT ( 'NONE',  ( 2.546103534247748712, 3.000000000000000000, -12.55526518755974585 ) ) ;
#7723 = CARTESIAN_POINT ( 'NONE',  ( -11.11702303352192445, 3.000000000000000000, 8.914835885878272137 ) ) ;
#7724 = PLANE ( 'NONE',  #1210 ) ;
#7725 = ORIENTED_EDGE ( 'NONE', *, *, #6394, .F. ) ;
#7726 = DIRECTION ( 'NONE',  ( 0.000000000000000000, 1.000000000000000000, 0.000000000000000000 ) ) ;
#7727 = AXIS2_PLACEMENT_3D ( 'NONE', #8301, #6240, #2109 ) ;
#7728 = VERTEX_POINT ( 'NONE', #6714 ) ;
#7729 = ORIENTED_EDGE ( 'NONE', *, *, #11579, .F. ) ;
#7730 = ORIENTED_EDGE ( 'NONE', *, *, #12949, .T. ) ;
#7731 = EDGE_CURVE ( 'NONE', #1266, #7435, #1145, .T. ) ;
#7732 = FACE_OUTER_BOUND ( 'NONE', #8637, .T. ) ;
#7733 = CLOSED_SHELL ( 'NONE', ( #3366, #10367, #4961, #1647, #6569, #1096, #7046, #5978, #7747, #9663, #9020, #10373, #7837, #13158, #1431, #7266, #2955, #3839, #11653, #11925, #8752, #6834, #8820, #10148, #11569, #537, #3461, #8431, #11959, #4724, #6500, #9462, #2260, #4227, #9962, #2465, #29, #7375, #9829, #11644, #10630, #2873, #9864, #11984, #4847, #13320, #12460, #2581, #10726, #12658 ) ) ;
#7734 = CARTESIAN_POINT ( 'NONE',  ( 11.70905276178455878, 0.000000000000000000, -9.375397774054460953 ) ) ;
#7735 = DIRECTION ( 'NONE',  ( -0.000000000000000000, -1.000000000000000000, -0.000000000000000000 ) ) ;
#7736 = CARTESIAN_POINT ( 'NONE',  ( 11.48836750521728511, 0.000000000000000000, 8.430890348300561499 ) ) ;
#7737 = CARTESIAN_POINT ( 'NONE',  ( 2.161962830978694683, 3.000000000000000000, -14.08504230442587790 ) ) ;
#7738 = CARTESIAN_POINT ( 'NONE',  ( 9.250000000000003553, 2.750000000000000888, -10.00000000000000178 ) ) ;
#7739 = ORIENTED_EDGE ( 'NONE', *, *, #9942, .T. ) ;
#7740 = VECTOR ( 'NONE', #11791, 1000.000000000000000 ) ;
#7741 = ORIENTED_EDGE ( 'NONE', *, *, #6528, .F. ) ;
#7742 = VECTOR ( 'NONE', #5072, 1000.000000000000000 ) ;
#7743 = CIRCLE ( 'NONE', #7526, 1.000000000000000888 ) ;
#7744 = CARTESIAN_POINT ( 'NONE',  ( -5.452638258930639914, 0.000000000000000000, -13.97385902380748313 ) ) ;
#7745 = B_SPLINE_SURFACE_WITH_KNOTS ( 'NONE', 3, 1, ( 
 ( #2224, #9797 ),
 ( #8691, #11866 ),
 ( #373, #4564 ),
 ( #6427, #10639 ) ),
 .UNSPECIFIED., .F., .F., .F.,
 ( 4, 4 ),
 ( 2, 2 ),
 ( 0.1276832474596270861, 1.000000000000000000 ),
 ( 0.000000000000000000, 1.000000000000000000 ),
 .UNSPECIFIED. ) ;
#7746 = EDGE_CURVE ( 'NONE', #8499, #6668, #12600, .T. ) ;
#7747 = ADVANCED_FACE ( 'NONE', ( #12856 ), #2905, .T. ) ;
#7748 = ORIENTED_EDGE ( 'NONE', *, *, #1445, .T. ) ;
#7749 = FACE_OUTER_BOUND ( 'NONE', #2319, .T. ) ;
#7750 = CARTESIAN_POINT ( 'NONE',  ( 6.506620931068708202, 0.000000000000000000, 10.18979803820052155 ) ) ;
#7751 = AXIS2_PLACEMENT_3D ( 'NONE', #1502, #6534, #402 ) ;
#7752 = EDGE_CURVE ( 'NONE', #1864, #8421, #484, .T. ) ;
#7753 = CARTESIAN_POINT ( 'NONE',  ( 1.132798289211301698E-15, 0.000000000000000000, -9.250000000000000000 ) ) ;
#7754 = CIRCLE ( 'NONE', #6655, 1.000000000000000888 ) ;
#7755 = EDGE_CURVE ( 'NONE', #7331, #3742, #10645, .T. ) ;
#7756 = AXIS2_PLACEMENT_3D ( 'NONE', #9456, #8348, #13468 ) ;
#7757 = CARTESIAN_POINT ( 'NONE',  ( 4.652003457867571967, 0.000000000000000000, -6.437678087145717321 ) ) ;
#7758 = DIRECTION ( 'NONE',  ( -0.000000000000000000, -1.000000000000000000, -0.000000000000000000 ) ) ;
#7759 = CARTESIAN_POINT ( 'NONE',  ( -8.352599575481674421, 3.000000000000000000, 31.00000000000000000 ) ) ;
#7760 = CARTESIAN_POINT ( 'NONE',  ( -7.500000000000000000, 3.000000000000000000, 0.000000000000000000 ) ) ;
#7761 = CARTESIAN_POINT ( 'NONE',  ( 0.000000000000000000, 3.000000000000000000, 0.000000000000000000 ) ) ;
#7762 = VERTEX_POINT ( 'NONE', #7060 ) ;
#7763 = ORIENTED_EDGE ( 'NONE', *, *, #1854, .F. ) ;
#7764 = ORIENTED_EDGE ( 'NONE', *, *, #2780, .T. ) ;
#7765 = VECTOR ( 'NONE', #11500, 1000.000000000000000 ) ;
#7767 = ORIENTED_EDGE ( 'NONE', *, *, #4929, .T. ) ;
#7766 = B_SPLINE_CURVE_WITH_KNOTS ( 'NONE', 3,
 ( #4588, #1099, #5296, #4268 ),
 .UNSPECIFIED., .F., .F.,
 ( 4, 4 ),
 ( 0.000000000000000000, 0.5855695330273008592 ),
 .UNSPECIFIED. ) ;
#7768 = CARTESIAN_POINT ( 'NONE',  ( -6.506620931068619385, 0.000000000000000000, -10.18979803820057306 ) ) ;
#7769 = EDGE_CURVE ( 'NONE', #5694, #912, #6994, .T. ) ;
#7770 = EDGE_LOOP ( 'NONE', ( #9369, #774, #3394, #9628 ) ) ;
#7771 = FACE_OUTER_BOUND ( 'NONE', #8515, .T. ) ;
#7772 = ADVANCED_FACE ( 'NONE', ( #9186 ), #10980, .T. ) ;
#7773 = DIRECTION ( 'NONE',  ( -0.000000000000000000, -1.000000000000000000, -0.000000000000000000 ) ) ;
#7774 = LINE ( 'NONE', #2546, #3393 ) ;
#7775 = PRODUCT_DEFINITION_SHAPE ( 'NONE', 'NONE',  #1605 ) ;
#7776 = AXIS2_PLACEMENT_3D ( 'NONE', #11707, #4342, #5369 ) ;
#7777 = CYLINDRICAL_SURFACE ( 'NONE', #10387, 12.08999999999737440 ) ;
#7778 = DIRECTION ( 'NONE',  ( -0.9893737785712105604, 0.000000000000000000, 0.1453943818575020863 ) ) ;
#7779 = VERTEX_POINT ( 'NONE', #1759 ) ;
#7780 = DIRECTION ( 'NONE',  ( 0.000000000000000000, 1.000000000000000000, 0.000000000000000000 ) ) ;
#7781 = VERTEX_POINT ( 'NONE', #593 ) ;
#7782 = ORIENTED_EDGE ( 'NONE', *, *, #2472, .F. ) ;
#7783 = FACE_OUTER_BOUND ( 'NONE', #11786, .T. ) ;
#7784 = EDGE_CURVE ( 'NONE', #9896, #8568, #12395, .T. ) ;
#7785 = EDGE_CURVE ( 'NONE', #3437, #11402, #10084, .T. ) ;
#7786 = VERTEX_POINT ( 'NONE', #11127 ) ;
#7787 = CIRCLE ( 'NONE', #773, 12.08999999999737440 ) ;
#7788 = ORIENTED_EDGE ( 'NONE', *, *, #5730, .T. ) ;
#7789 = CARTESIAN_POINT ( 'NONE',  ( 2.830255545554135832, 0.000000000000000000, -12.68816982652952596 ) ) ;
#7790 = CARTESIAN_POINT ( 'NONE',  ( -13.82336506795094522, 0.000000000000000000, -0.6724118135761603110 ) ) ;
#7791 = DIRECTION ( 'NONE',  ( 0.000000000000000000, 1.000000000000000000, 0.000000000000000000 ) ) ;
#7792 = CARTESIAN_POINT ( 'NONE',  ( -8.100301009650792139, 9.000000000000000000, -2.575873357339267589 ) ) ;
#7793 = CARTESIAN_POINT ( 'NONE',  ( -14.82803603298502360, 3.000000000000000000, -2.264806262022826644 ) ) ;
#7794 = DIRECTION ( 'NONE',  ( -3.469446951953614189E-15, -1.000000000000000000, 0.000000000000000000 ) ) ;
#7795 = VERTEX_POINT ( 'NONE', #3883 ) ;
#7796 = PRESENTATION_LAYER_ASSIGNMENT (  '', '', ( #11764 ) ) ;
#7797 = CARTESIAN_POINT ( 'NONE',  ( -13.97385902380755240, 3.000000000000000000, -5.452638258930474713 ) ) ;
#7798 = AXIS2_PLACEMENT_3D ( 'NONE', #11801, #9795, #11937 ) ;
#7799 = EDGE_LOOP ( 'NONE', ( #610, #1265, #7407, #3053 ) ) ;
#7800 = ORIENTED_EDGE ( 'NONE', *, *, #1148, .F. ) ;
#7801 = ORIENTED_EDGE ( 'NONE', *, *, #12254, .F. ) ;
#7802 = CARTESIAN_POINT ( 'NONE',  ( 8.430890348300625448, 0.000000000000000000, 11.48836750521723893 ) ) ;
#7803 = COLOUR_RGB ( '',0.7803921568627451011, 0.7607843137254901578, 0.7411764705882353255 ) ;
#7804 = CARTESIAN_POINT ( 'NONE',  ( 4.056222772158357692, 0.000000000000000000, -12.16218796965919680 ) ) ;
#7805 = CARTESIAN_POINT ( 'NONE',  ( -14.08504230442586369, 3.000000000000000000, 2.161962830978784389 ) ) ;
#7806 = CARTESIAN_POINT ( 'NONE',  ( -12.51336114795298471, 0.000000000000000000, -3.542894103880322998 ) ) ;
#7807 = FACE_OUTER_BOUND ( 'NONE', #56, .T. ) ;
#7808 = CARTESIAN_POINT ( 'NONE',  ( 0.000000000000000000, 2.900000000000000355, 0.000000000000000000 ) ) ;
#7809 = DIRECTION ( 'NONE',  ( 0.000000000000000000, 0.000000000000000000, -1.000000000000000000 ) ) ;
#7810 = CARTESIAN_POINT ( 'NONE',  ( 13.27898586450067242, 3.000000000000000000, -5.170206418547655502 ) ) ;
#7811 = EDGE_LOOP ( 'NONE', ( #7990, #2739, #94, #9580 ) ) ;
#7812 = EDGE_CURVE ( 'NONE', #5535, #43, #7538, .T. ) ;
#7813 = AXIS2_PLACEMENT_3D ( 'NONE', #2674, #763, #11013 ) ;
#7814 = EDGE_LOOP ( 'NONE', ( #11938, #8781, #2534, #2680 ) ) ;
#7815 = ORIENTED_EDGE ( 'NONE', *, *, #1799, .T. ) ;
#7816 = DIRECTION ( 'NONE',  ( 0.000000000000000000, 1.000000000000000000, -0.000000000000000000 ) ) ;
#7817 = CARTESIAN_POINT ( 'NONE',  ( 0.000000000000000000, 3.000000000000000000, 0.000000000000000000 ) ) ;
#7818 = DIRECTION ( 'NONE',  ( 0.000000000000000000, 1.000000000000000000, 0.000000000000000000 ) ) ;
#7819 = DIRECTION ( 'NONE',  ( -0.000000000000000000, -1.000000000000000000, -0.000000000000000000 ) ) ;
#7820 = CARTESIAN_POINT ( 'NONE',  ( 3.469446951953614189E-15, 3.000000000000000000, -7.049999999999999822 ) ) ;
#7821 = CARTESIAN_POINT ( 'NONE',  ( 0.000000000000000000, 3.000000000000000000, 0.000000000000000000 ) ) ;
#7822 = CARTESIAN_POINT ( 'NONE',  ( 52.12339130828321032, 3.000000000000000000, -4.353525159591052685 ) ) ;
#7823 = EDGE_CURVE ( 'NONE', #1734, #10022, #13187, .T. ) ;
#7824 = LINE ( 'NONE', #1565, #9103 ) ;
#7825 = ADVANCED_FACE ( 'NONE', ( #8149 ), #726, .F. ) ;
#7826 = DIRECTION ( 'NONE',  ( -1.000000000000000000, 3.469446951953610639E-15, 2.602085213965210149E-16 ) ) ;
#7827 = ORIENTED_EDGE ( 'NONE', *, *, #4220, .T. ) ;
#7828 = ORIENTED_EDGE ( 'NONE', *, *, #7133, .F. ) ;
#7829 = ORIENTED_EDGE ( 'NONE', *, *, #6917, .F. ) ;
#7830 = CARTESIAN_POINT ( 'NONE',  ( 1.132798289211301698E-15, -3.000000000000000000, -9.250000000000000000 ) ) ;
#7831 = ADVANCED_FACE ( 'NONE', ( #4923 ), #8617, .F. ) ;
#7832 = VERTEX_POINT ( 'NONE', #8909 ) ;
#7833 = CARTESIAN_POINT ( 'NONE',  ( 5.733772933379474246, 0.000000000000000000, -13.04554897075799502 ) ) ;
#7834 = DIRECTION ( 'NONE',  ( 1.000000000000000000, 0.000000000000000000, 0.000000000000000000 ) ) ;
#7835 = DIRECTION ( 'NONE',  ( 0.000000000000000000, 1.000000000000000000, 0.000000000000000000 ) ) ;
#7836 = CARTESIAN_POINT ( 'NONE',  ( 6.970598036433451661, 3.000000000000000000, -10.97318381393796294 ) ) ;
#7837 = ADVANCED_FACE ( 'NONE', ( #3740 ), #6030, .F. ) ;
#7838 = CARTESIAN_POINT ( 'NONE',  ( -13.97385902380755240, 3.000000000000000000, -5.452638258930474713 ) ) ;
#7839 = CARTESIAN_POINT ( 'NONE',  ( -5.741477348071430065, 3.000000000000000000, -13.86115248177175374 ) ) ;
#7840 = EDGE_LOOP ( 'NONE', ( #5691, #8739, #709, #6328 ) ) ;
#7841 = FACE_OUTER_BOUND ( 'NONE', #6565, .T. ) ;
#7842 = ORIENTED_EDGE ( 'NONE', *, *, #9921, .F. ) ;
#7843 = EDGE_CURVE ( 'NONE', #5502, #9963, #803, .T. ) ;
#7844 = ORIENTED_EDGE ( 'NONE', *, *, #4626, .F. ) ;
#7845 = DIRECTION ( 'NONE',  ( -3.469446951953610639E-15, -1.000000000000000000, -2.891205793294675861E-16 ) ) ;
#7846 = ADVANCED_FACE ( 'NONE', ( #2641 ), #6848, .F. ) ;
#7847 = ADVANCED_BREP_SHAPE_REPRESENTATION ( '', ( #8440, #10007 ), #5843 ) ;
#7848 = ORIENTED_EDGE ( 'NONE', *, *, #8846, .T. ) ;
#7849 = EDGE_LOOP ( 'NONE', ( #469, #11633, #7782, #8220 ) ) ;
#7850 = CARTESIAN_POINT ( 'NONE',  ( 0.000000000000000000, 9.000000000000000000, 0.000000000000000000 ) ) ;
#7851 = PLANE ( 'NONE',  #12171 ) ;
#7852 = CARTESIAN_POINT ( 'NONE',  ( -5.526615004551211463, 0.000000000000000000, -4.866191470063547797 ) ) ;
#7853 = CARTESIAN_POINT ( 'NONE',  ( -13.50845331674225847, 3.000000000000000000, 1.119409668803372115 ) ) ;
#7854 = CARTESIAN_POINT ( 'NONE',  ( 8.914835885878220623, 3.000000000000000000, -11.11702303352196708 ) ) ;
#7855 = DIRECTION ( 'NONE',  ( 0.000000000000000000, 1.000000000000000000, -0.000000000000000000 ) ) ;
#7856 = ORIENTED_EDGE ( 'NONE', *, *, #5242, .T. ) ;
#7857 = CARTESIAN_POINT ( 'NONE',  ( -6.217402469309367241, 0.000000000000000000, -13.03533457366727610 ) ) ;
#7858 = B_SPLINE_SURFACE_WITH_KNOTS ( 'NONE', 3, 1, ( 
 ( #6638, #10845 ),
 ( #1212, #3606 ),
 ( #12917, #13049 ),
 ( #5402, #11748 ) ),
 .UNSPECIFIED., .F., .F., .F.,
 ( 4, 4 ),
 ( 2, 2 ),
 ( 0.1276832474596284739, 1.000000000000000000 ),
 ( 0.000000000000000000, 1.000000000000000000 ),
 .UNSPECIFIED. ) ;
#7859 = VERTEX_POINT ( 'NONE', #6292 ) ;
#7860 = VERTEX_POINT ( 'NONE', #4155 ) ;
#7861 = ORIENTED_EDGE ( 'NONE', *, *, #4731, .F. ) ;
#7862 = CARTESIAN_POINT ( 'NONE',  ( 0.000000000000000000, 0.000000000000000000, 0.000000000000000000 ) ) ;
#7863 = LINE ( 'NONE', #436, #4506 ) ;
#7864 = LINE ( 'NONE', #9033, #9295 ) ;
#7865 = LINE ( 'NONE', #10145, #4611 ) ;
#7866 = FACE_OUTER_BOUND ( 'NONE', #13018, .T. ) ;
#7867 = B_SPLINE_CURVE_WITH_KNOTS ( 'NONE', 3,
 ( #1530, #10130, #4770, #4901 ),
 .UNSPECIFIED., .F., .F.,
 ( 4, 4 ),
 ( 0.000000000000000000, 0.8452273900860258760 ),
 .UNSPECIFIED. ) ;
#7868 = ITEM_DEFINED_TRANSFORMATION ( 'NONE', 'NONE', #3207,  #10007 ) ;
#7869 = CARTESIAN_POINT ( 'NONE',  ( 0.000000000000000000, 3.000000000000000000, 0.000000000000000000 ) ) ;
#7870 = ADVANCED_FACE ( 'NONE', ( #4218, #9401 ), #114, .T. ) ;
#7871 = CARTESIAN_POINT ( 'NONE',  ( -4.679611352264966051, -1.694065894508600678E-18, -6.417326716594978997 ) ) ;
#7872 = CARTESIAN_POINT ( 'NONE',  ( 12.03251085770905959, 3.000000000000000000, 3.999999998926332179 ) ) ;
#7873 = ADVANCED_FACE ( 'NONE', ( #11337 ), #12517, .T. ) ;
#7874 = CARTESIAN_POINT ( 'NONE',  ( -13.28140389626389783, 3.000000000000000000, -1.567980996311402420 ) ) ;
#7875 = CARTESIAN_POINT ( 'NONE',  ( -6.749999880766614169, 9.000000000000000000, -0.001268720102703135150 ) ) ;
#7876 = ORIENTED_EDGE ( 'NONE', *, *, #6674, .F. ) ;
#7877 = ORIENTED_EDGE ( 'NONE', *, *, #5729, .F. ) ;
#7878 = ORIENTED_EDGE ( 'NONE', *, *, #2374, .F. ) ;
#7879 = CARTESIAN_POINT ( 'NONE',  ( 1.557181465540672161, 3.000000000000000000, -14.16466328168010591 ) ) ;
#7880 = DIRECTION ( 'NONE',  ( -0.000000000000000000, -1.000000000000000000, -0.000000000000000000 ) ) ;
#7881 = CARTESIAN_POINT ( 'NONE',  ( -5.999999999999991118, 3.000000000000000000, 25.50000000000000000 ) ) ;
#7882 = CARTESIAN_POINT ( 'NONE',  ( -0.5501230721523990841, 3.000000000000000000, -12.98835496148299384 ) ) ;
#7883 = CARTESIAN_POINT ( 'NONE',  ( 5.504794476853524188, 9.000000000000000000, -4.890042597913815570 ) ) ;
#7884 = DIRECTION ( 'NONE',  ( 0.000000000000000000, 1.000000000000000000, -0.000000000000000000 ) ) ;
#7885 = DIRECTION ( 'NONE',  ( -0.000000000000000000, -1.000000000000000000, -0.000000000000000000 ) ) ;
#7886 = LINE ( 'NONE', #3758, #8210 ) ;
#7887 = ORIENTED_EDGE ( 'NONE', *, *, #4410, .F. ) ;
#7888 = ORIENTED_EDGE ( 'NONE', *, *, #13323, .F. ) ;
#7889 = ORIENTED_EDGE ( 'NONE', *, *, #12332, .T. ) ;
#7890 = DIRECTION ( 'NONE',  ( 0.000000000000000000, 0.000000000000000000, -1.000000000000000000 ) ) ;
#7891 = ORIENTED_EDGE ( 'NONE', *, *, #4572, .T. ) ;
#7892 = AXIS2_PLACEMENT_3D ( 'NONE', #4382, #2055, #4322 ) ;
#7893 = EDGE_CURVE ( 'NONE', #3759, #8307, #10141, .T. ) ;
#7894 = CARTESIAN_POINT ( 'NONE',  ( 10.18987059060247269, 3.000000000000000000, 6.506507307819714647 ) ) ;
#7895 = DIRECTION ( 'NONE',  ( 0.8254356770911533969, 1.772319007508385941E-15, 0.5644961850934593350 ) ) ;
#7896 = EDGE_CURVE ( 'NONE', #5259, #10212, #1600, .T. ) ;
#7897 = CARTESIAN_POINT ( 'NONE',  ( 6.554160776451332104, 0.000000000000000000, -1.614148852004323231 ) ) ;
#7898 = CARTESIAN_POINT ( 'NONE',  ( -5.496871281090180972, 9.000000000000000000, 4.899765193453235135 ) ) ;
#7899 = DIRECTION ( 'NONE',  ( 0.000000000000000000, 0.000000000000000000, -1.000000000000000000 ) ) ;
#7900 = CARTESIAN_POINT ( 'NONE',  ( -10.97318381393799136, 0.000000000000000000, -6.970598036433411693 ) ) ;
#7901 = DIRECTION ( 'NONE',  ( 0.000000000000000000, 0.000000000000000000, -1.000000000000000000 ) ) ;
#7902 = B_SPLINE_SURFACE_WITH_KNOTS ( 'NONE', 3, 1, ( 
 ( #4622, #3718 ),
 ( #12217, #703 ),
 ( #8954, #2496 ),
 ( #11027, #4696 ) ),
 .UNSPECIFIED., .F., .F., .F.,
 ( 4, 4 ),
 ( 2, 2 ),
 ( 0.000000000000000000, 0.8724294488011758997 ),
 ( 0.000000000000000000, 1.000000000000000000 ),
 .UNSPECIFIED. ) ;
#7903 = ORIENTED_EDGE ( 'NONE', *, *, #607, .T. ) ;
#7904 = CARTESIAN_POINT ( 'NONE',  ( -7.500000000000000000, 3.000000000000000000, 0.000000000000000000 ) ) ;
#7905 = AXIS2_PLACEMENT_3D ( 'NONE', #10512, #7616, #13549 ) ;
#7906 = VERTEX_POINT ( 'NONE', #3194 ) ;
#7907 = CIRCLE ( 'NONE', #9007, 3.100000000000000533 ) ;
#7908 = ORIENTED_EDGE ( 'NONE', *, *, #2953, .T. ) ;
#7909 = CARTESIAN_POINT ( 'NONE',  ( -7.065816209474154341, 0.000000000000000000, 10.69794375946289833 ) ) ;
#7910 = VERTEX_POINT ( 'NONE', #2997 ) ;
#7911 = EDGE_CURVE ( 'NONE', #7608, #3702, #11401, .T. ) ;
#7912 = ORIENTED_EDGE ( 'NONE', *, *, #458, .T. ) ;
#7913 = EDGE_CURVE ( 'NONE', #1800, #7218, #7330, .T. ) ;
#7914 = DIRECTION ( 'NONE',  ( 0.000000000000000000, 1.000000000000000000, 0.000000000000000000 ) ) ;
#7915 = VECTOR ( 'NONE', #12375, 1000.000000000000000 ) ;
#7916 = APPLICATION_CONTEXT ( 'automotive_design' ) ;
#7917 = DIRECTION ( 'NONE',  ( -0.000000000000000000, -1.000000000000000000, -0.000000000000000000 ) ) ;
#7918 = DIRECTION ( 'NONE',  ( 0.000000000000000000, 0.000000000000000000, 1.000000000000000000 ) ) ;
#7919 = AXIS2_PLACEMENT_3D ( 'NONE', #6624, #10824, #2218 ) ;
#7920 = EDGE_CURVE ( 'NONE', #10584, #8551, #9655, .T. ) ;
#7921 = CARTESIAN_POINT ( 'NONE',  ( -8.430890348300632553, 3.000000000000000000, -11.48836750521723538 ) ) ;
#7922 = EDGE_CURVE ( 'NONE', #5839, #11792, #12022, .T. ) ;
#7923 = DIRECTION ( 'NONE',  ( -0.000000000000000000, -1.000000000000000000, -0.000000000000000000 ) ) ;
#7924 = CARTESIAN_POINT ( 'NONE',  ( -0.5400000000008023937, 3.000000000000000000, -12.07793442604883971 ) ) ;
#7925 = ORIENTED_EDGE ( 'NONE', *, *, #11133, .F. ) ;
#7926 = DIRECTION ( 'NONE',  ( 0.000000000000000000, 0.000000000000000000, -1.000000000000000000 ) ) ;
#7927 = EDGE_LOOP ( 'NONE', ( #8469, #7445, #7336, #9404, #808, #7000 ) ) ;
#7928 = ORIENTED_EDGE ( 'NONE', *, *, #12521, .T. ) ;
#7929 = AXIS2_PLACEMENT_3D ( 'NONE', #1257, #231, #5773 ) ;
#7930 = AXIS2_PLACEMENT_3D ( 'NONE', #1446, #2603, #11081 ) ;
#7931 = ORIENTED_EDGE ( 'NONE', *, *, #8235, .T. ) ;
#7932 = EDGE_CURVE ( 'NONE', #9350, #8654, #6361, .T. ) ;
#7933 = CARTESIAN_POINT ( 'NONE',  ( 41.29994854050690378, 0.000000000000000000, -6.141175130212632283 ) ) ;
#7934 = CARTESIAN_POINT ( 'NONE',  ( -5.571313494980134173, 0.000000000000000000, 10.72979803820131295 ) ) ;
#7935 = ADVANCED_FACE ( 'NONE', ( #2098 ), #12809, .F. ) ;
#7936 = DIRECTION ( 'NONE',  ( -0.000000000000000000, -1.000000000000000000, -0.000000000000000000 ) ) ;
#7937 = CARTESIAN_POINT ( 'NONE',  ( 6.509732753943064054, 0.000000000000000000, -3.441899519755141412 ) ) ;
#7938 = DIRECTION ( 'NONE',  ( 0.6291930273683166153, 0.000000000000000000, -0.7772490812545826966 ) ) ;
#7939 = SHAPE_REPRESENTATION ( 'link', ( #10007 ), #1673 ) ;
#7940 = CARTESIAN_POINT ( 'NONE',  ( -8.795158114916672432, 0.000000000000000000, -9.573149624528774382 ) ) ;
#7941 = ADVANCED_FACE ( 'NONE', ( #10295 ), #8290, .F. ) ;
#7942 = VECTOR ( 'NONE', #5817, 1000.000000000000000 ) ;
#7943 = CARTESIAN_POINT ( 'NONE',  ( -5.999999999999991118, 3.000000000000000000, 27.00000000000000000 ) ) ;
#7944 = CARTESIAN_POINT ( 'NONE',  ( 28.56494132578241008, 0.000000000000000000, -0.9541491613812155270 ) ) ;
#7945 = VECTOR ( 'NONE', #5336, 1000.000000000000000 ) ;
#7946 = CARTESIAN_POINT ( 'NONE',  ( 9.250000000000003553, 2.750000000000000888, 10.00000000000000000 ) ) ;
#7947 = DIRECTION ( 'NONE',  ( 0.000000000000000000, 0.000000000000000000, -1.000000000000000000 ) ) ;
#7948 = ORIENTED_EDGE ( 'NONE', *, *, #413, .F. ) ;
#7949 = VERTEX_POINT ( 'NONE', #9250 ) ;
#7950 = CIRCLE ( 'NONE', #2026, 1.000000000000000888 ) ;
#7951 = EDGE_LOOP ( 'NONE', ( #9131, #9027, #5584, #10831 ) ) ;
#7952 = CARTESIAN_POINT ( 'NONE',  ( 6.506507307819716424, 3.000000000000000000, -10.18987059060247269 ) ) ;
#7953 = CARTESIAN_POINT ( 'NONE',  ( 7.077546079049268357, 3.000000000000000000, 10.67828022838850544 ) ) ;
#7954 = CARTESIAN_POINT ( 'NONE',  ( 0.000000000000000000, 1.000000000000000000, 0.000000000000000000 ) ) ;
#7955 = ADVANCED_FACE ( 'NONE', ( #1062 ), #39, .T. ) ;
#7956 = LINE ( 'NONE', #11136, #12552 ) ;
#7957 = CARTESIAN_POINT ( 'NONE',  ( 6.970598036433451661, 0.000000000000000000, -10.97318381393796294 ) ) ;
#7958 = B_SPLINE_CURVE_WITH_KNOTS ( 'NONE', 2,
 ( #2890, #9084, #9220 ),
 .UNSPECIFIED., .F., .F.,
 ( 3, 3 ),
 ( 0.000000000000000000, 1.000000000000000000 ),
 .UNSPECIFIED. ) ;
#7959 = B_SPLINE_SURFACE_WITH_KNOTS ( 'NONE', 3, 1, ( 
 ( #2545, #8544 ),
 ( #7459, #11659 ),
 ( #1193, #1927 ),
 ( #8049, #7976 ) ),
 .UNSPECIFIED., .F., .F., .F.,
 ( 4, 4 ),
 ( 2, 2 ),
 ( 0.000000000000000000, 0.8452273900860258760 ),
 ( 0.000000000000000000, 1.000000000000000000 ),
 .UNSPECIFIED. ) ;
#7960 = CIRCLE ( 'NONE', #6419, 8.500000000000000000 ) ;
#7961 = CARTESIAN_POINT ( 'NONE',  ( 0.000000000000000000, 3.000000000000000000, -1.500000000000000222 ) ) ;
#7962 = AXIS2_PLACEMENT_3D ( 'NONE', #13364, #7413, #10515 ) ;
#7963 = CARTESIAN_POINT ( 'NONE',  ( -8.222660081691577361, 3.000000000000000000, -5.549999999999999822 ) ) ;
#7964 = FACE_OUTER_BOUND ( 'NONE', #13208, .T. ) ;
#7965 = EDGE_LOOP ( 'NONE', ( #7159, #12966, #671, #2612 ) ) ;
#7966 = ORIENTED_EDGE ( 'NONE', *, *, #9632, .T. ) ;
#7967 = EDGE_LOOP ( 'NONE', ( #9008, #8423, #10018, #10998 ) ) ;
#7968 = CARTESIAN_POINT ( 'NONE',  ( 30.79786191028635400, 0.000000000000000000, -6.999232361977355765 ) ) ;
#7969 = ORIENTED_EDGE ( 'NONE', *, *, #9004, .T. ) ;
#7970 = VECTOR ( 'NONE', #9236, 1000.000000000000000 ) ;
#7971 = AXIS2_PLACEMENT_3D ( 'NONE', #2153, #3108, #5250 ) ;
#7972 = AXIS2_PLACEMENT_3D ( 'NONE', #576, #9101, #3869 ) ;
#7973 = CARTESIAN_POINT ( 'NONE',  ( 6.506620931068707314, 3.000000000000000000, 10.18979803820051622 ) ) ;
#7974 = CARTESIAN_POINT ( 'NONE',  ( 59.20906036370015357, 38.33135765298362685, 9.098535593488138673 ) ) ;
#7975 = DIRECTION ( 'NONE',  ( -0.000000000000000000, -1.000000000000000000, -0.000000000000000000 ) ) ;
#7976 = CARTESIAN_POINT ( 'NONE',  ( -11.52666717836884125, 0.000000000000000000, -3.647470871583627705 ) ) ;
#7977 = DIRECTION ( 'NONE',  ( 0.000000000000000000, 1.000000000000000000, 0.000000000000000000 ) ) ;
#7978 = DIRECTION ( 'NONE',  ( 0.000000000000000000, 0.000000000000000000, 1.000000000000000000 ) ) ;
#7979 = CARTESIAN_POINT ( 'NONE',  ( -1.161309641800940540, 0.000000000000000000, -7.856984441350959969 ) ) ;
#7980 = ORIENTED_EDGE ( 'NONE', *, *, #151, .F. ) ;
#7981 = VECTOR ( 'NONE', #6261, 1000.000000000000000 ) ;
#7982 = CARTESIAN_POINT ( 'NONE',  ( 19.60942157306000766, 3.000000000000000000, 14.05941790610251374 ) ) ;
#7983 = AXIS2_PLACEMENT_3D ( 'NONE', #1878, #5098, #13442 ) ;
#7984 = ORIENTED_EDGE ( 'NONE', *, *, #5488, .F. ) ;
#7985 = EDGE_CURVE ( 'NONE', #9002, #1142, #12457, .T. ) ;
#7986 = ORIENTED_EDGE ( 'NONE', *, *, #11810, .F. ) ;
#7987 = DIRECTION ( 'NONE',  ( 1.000000000000000000, 0.000000000000000000, 0.000000000000000000 ) ) ;
#7988 = ORIENTED_EDGE ( 'NONE', *, *, #6604, .T. ) ;
#7989 = DIRECTION ( 'NONE',  ( -0.000000000000000000, -1.000000000000000000, -0.000000000000000000 ) ) ;
#7990 = ORIENTED_EDGE ( 'NONE', *, *, #12040, .T. ) ;
#7991 = DIRECTION ( 'NONE',  ( 0.000000000000000000, 0.000000000000000000, 1.000000000000000000 ) ) ;
#7992 = TOROIDAL_SURFACE ( 'NONE', #749, 3.399999999999999911, 0.1000000000000000056 ) ;
#7993 = CIRCLE ( 'NONE', #2064, 1.600000000000004086 ) ;
#7994 = VECTOR ( 'NONE', #8238, 1000.000000000000000 ) ;
#7995 = FACE_OUTER_BOUND ( 'NONE', #5092, .T. ) ;
#7996 = FACE_OUTER_BOUND ( 'NONE', #9814, .T. ) ;
#7997 = CARTESIAN_POINT ( 'NONE',  ( -0.5400000000007666445, 0.000000000000000000, -12.07793442604883793 ) ) ;
#7998 = CARTESIAN_POINT ( 'NONE',  ( 8.158551673544282679, 3.000000000000000000, -8.922226997226884393 ) ) ;
#7999 = DIRECTION ( 'NONE',  ( 0.000000000000000000, 0.000000000000000000, 1.000000000000000000 ) ) ;
#8000 = ORIENTED_EDGE ( 'NONE', *, *, #8422, .T. ) ;
#8001 = CARTESIAN_POINT ( 'NONE',  ( 9.250000000000001776, 0.000000000000000000, 10.00000000000000000 ) ) ;
#8002 = ORIENTED_EDGE ( 'NONE', *, *, #5571, .T. ) ;
#8003 = VERTEX_POINT ( 'NONE', #10565 ) ;
#8004 = AXIS2_PLACEMENT_3D ( 'NONE', #4401, #8591, #3363 ) ;
#8005 = DIRECTION ( 'NONE',  ( -2.312964634635735561E-15, -1.000000000000000000, 0.000000000000000000 ) ) ;
#8006 = AXIS2_PLACEMENT_3D ( 'NONE', #11039, #2573, #8009 ) ;
#8007 = ORIENTED_EDGE ( 'NONE', *, *, #3956, .F. ) ;
#8008 = EDGE_CURVE ( 'NONE', #12983, #7207, #1002, .T. ) ;
#8009 = DIRECTION ( 'NONE',  ( 0.000000000000000000, 0.000000000000000000, -1.000000000000000000 ) ) ;
#8010 = CARTESIAN_POINT ( 'NONE',  ( 8.922136023539611216, 3.000000000000000000, -8.158651161643899030 ) ) ;
#8011 = CARTESIAN_POINT ( 'NONE',  ( 0.000000000000000000, 9.000000000000000000, 0.000000000000000000 ) ) ;
#8012 = CARTESIAN_POINT ( 'NONE',  ( -12.98835496148299207, 0.000000000000000000, 0.5501230721524459355 ) ) ;
#8013 = DIRECTION ( 'NONE',  ( -0.000000000000000000, -1.000000000000000000, -0.000000000000000000 ) ) ;
#8014 = CIRCLE ( 'NONE', #1198, 3.400000000000001243 ) ;
#8015 = CARTESIAN_POINT ( 'NONE',  ( 0.000000000000000000, 3.000000000000000000, 0.000000000000000000 ) ) ;
#8016 = CIRCLE ( 'NONE', #4267, 0.1000000000000000472 ) ;
#8017 = CARTESIAN_POINT ( 'NONE',  ( -9.573149624528719315, 3.000000000000000000, -8.795158114916407754 ) ) ;
#8018 = FACE_BOUND ( 'NONE', #12439, .T. ) ;
#8019 = CARTESIAN_POINT ( 'NONE',  ( 10.67828022838850366, 0.000000000000000000, -7.077546079049271022 ) ) ;
#8020 = DIRECTION ( 'NONE',  ( 0.000000000000000000, 0.000000000000000000, 1.000000000000000000 ) ) ;
#8021 = EDGE_CURVE ( 'NONE', #10212, #930, #3518, .T. ) ;
#8022 = ORIENTED_EDGE ( 'NONE', *, *, #8357, .T. ) ;
#8023 = ORIENTED_EDGE ( 'NONE', *, *, #535, .T. ) ;
#8024 = ORIENTED_EDGE ( 'NONE', *, *, #6998, .T. ) ;
#8025 = AXIS2_PLACEMENT_3D ( 'NONE', #11344, #6040, #11408 ) ;
#8026 = CIRCLE ( 'NONE', #13535, 14.25000000000000000 ) ;
#8027 = EDGE_CURVE ( 'NONE', #4625, #10097, #5660, .T. ) ;
#8028 = ORIENTED_EDGE ( 'NONE', *, *, #4678, .T. ) ;
#8029 = DIRECTION ( 'NONE',  ( 0.000000000000000000, 0.000000000000000000, -1.000000000000000000 ) ) ;
#8030 = CARTESIAN_POINT ( 'NONE',  ( 0.000000000000000000, 3.000000000000000000, 0.000000000000000000 ) ) ;
#8031 = CARTESIAN_POINT ( 'NONE',  ( 5.280889752749253319, 0.000000000000000000, -6.660495733750448899 ) ) ;
#8032 = DIRECTION ( 'NONE',  ( 0.000000000000000000, 1.000000000000000000, -0.000000000000000000 ) ) ;
#8033 = CARTESIAN_POINT ( 'NONE',  ( -2.928250210355484828, 0.000000000000000000, -13.52637830886140335 ) ) ;
#8034 = FACE_BOUND ( 'NONE', #1888, .T. ) ;
#8035 = AXIS2_PLACEMENT_3D ( 'NONE', #4198, #12815, #2202 ) ;
#8036 = EDGE_CURVE ( 'NONE', #911, #10812, #2916, .T. ) ;
#8037 = LINE ( 'NONE', #7963, #7146 ) ;
#8038 = EDGE_CURVE ( 'NONE', #9443, #7142, #9522, .T. ) ;
#8039 = CARTESIAN_POINT ( 'NONE',  ( 31.00000000000000000, 3.000000000000000000, 1.500000000000003997 ) ) ;
#8040 = VERTEX_POINT ( 'NONE', #1400 ) ;
#8041 = VERTEX_POINT ( 'NONE', #8549 ) ;
#8042 = ORIENTED_EDGE ( 'NONE', *, *, #4993, .T. ) ;
#8043 = CARTESIAN_POINT ( 'NONE',  ( -2.551540321038929007E-15, 2.000000000000000000, -7.000000000000000000 ) ) ;
#8044 = ORIENTED_EDGE ( 'NONE', *, *, #8764, .F. ) ;
#8045 = AXIS2_PLACEMENT_3D ( 'NONE', #7086, #1856, #2949 ) ;
#8046 = DIRECTION ( 'NONE',  ( -0.000000000000000000, -1.000000000000000000, -0.000000000000000000 ) ) ;
#8047 = DIRECTION ( 'NONE',  ( -0.8209917224599089236, -1.338292221737133534E-15, 0.5709400946266708354 ) ) ;
#8048 = CARTESIAN_POINT ( 'NONE',  ( -6.506507307819711095, 3.000000000000000000, 10.18987059060247624 ) ) ;
#8049 = CARTESIAN_POINT ( 'NONE',  ( -11.52666717836884125, 3.000000000000000000, -3.647470871583627705 ) ) ;
#8050 = DIRECTION ( 'NONE',  ( 1.224646799147353207E-16, 0.000000000000000000, -1.000000000000000000 ) ) ;
#8051 = B_SPLINE_CURVE_WITH_KNOTS ( 'NONE', 3,
 ( #1230, #10789, #8451, #6660 ),
 .UNSPECIFIED., .F., .F.,
 ( 4, 4 ),
 ( 0.000000000000000000, 0.8452273900860258760 ),
 .UNSPECIFIED. ) ;
#8052 = DIRECTION ( 'NONE',  ( 0.000000000000000000, 0.000000000000000000, 1.000000000000000000 ) ) ;
#8053 = EDGE_CURVE ( 'NONE', #7859, #1406, #11285, .T. ) ;
#8054 = FACE_OUTER_BOUND ( 'NONE', #5509, .T. ) ;
#8055 = EDGE_CURVE ( 'NONE', #12363, #11178, #3235, .T. ) ;
#8056 = EDGE_LOOP ( 'NONE', ( #7067, #13287, #305, #819 ) ) ;
#8057 =( NAMED_UNIT ( * ) PLANE_ANGLE_UNIT ( ) SI_UNIT ( $, .RADIAN. ) );
#8058 = ORIENTED_EDGE ( 'NONE', *, *, #7823, .F. ) ;
#8059 = UNCERTAINTY_MEASURE_WITH_UNIT (LENGTH_MEASURE( 1.000000000000000082E-05 ), #9635, 'distance_accuracy_value', 'NONE');
#8060 = VERTEX_POINT ( 'NONE', #7604 ) ;
#8061 = DIRECTION ( 'NONE',  ( 0.000000000000000000, 0.000000000000000000, 1.000000000000000000 ) ) ;
#8062 = B_SPLINE_CURVE_WITH_KNOTS ( 'NONE', 3,
 ( #11325, #918, #5190, #10142 ),
 .UNSPECIFIED., .F., .F.,
 ( 4, 4 ),
 ( 0.1276832474596304168, 1.000000000000000000 ),
 .UNSPECIFIED. ) ;
#8063 = ORIENTED_EDGE ( 'NONE', *, *, #9275, .T. ) ;
#8064 = CARTESIAN_POINT ( 'NONE',  ( 8.158551673544282679, 0.000000000000000000, -8.922226997226884393 ) ) ;
#8065 = ORIENTED_EDGE ( 'NONE', *, *, #7488, .T. ) ;
#8066 = DIRECTION ( 'NONE',  ( 0.000000000000000000, 0.000000000000000000, 1.000000000000000000 ) ) ;
#8067 =( LENGTH_UNIT ( ) NAMED_UNIT ( * ) SI_UNIT ( .MILLI., .METRE. ) );
#8068 = CARTESIAN_POINT ( 'NONE',  ( 6.017756925049591921, 0.000000000000000000, -11.52330688609011844 ) ) ;
#8069 = CARTESIAN_POINT ( 'NONE',  ( -1.557181465540760534, 0.000000000000000000, -14.16466328168009703 ) ) ;
#8070 = DIRECTION ( 'NONE',  ( 0.000000000000000000, 0.000000000000000000, 1.000000000000000000 ) ) ;
#8071 = CARTESIAN_POINT ( 'NONE',  ( 10.72973591378220704, 3.000000000000000000, -5.571433138827823761 ) ) ;
#8072 = FACE_OUTER_BOUND ( 'NONE', #11302, .T. ) ;
#8073 = ORIENTED_EDGE ( 'NONE', *, *, #8154, .F. ) ;
#8074 = CARTESIAN_POINT ( 'NONE',  ( -5.708888906988910605, 3.000000000000000000, 11.46847481510586597 ) ) ;
#8075 = VERTEX_POINT ( 'NONE', #176 ) ;
#8076 = ORIENTED_EDGE ( 'NONE', *, *, #8995, .F. ) ;
#8077 = CARTESIAN_POINT ( 'NONE',  ( -7.780961115628980629, 9.000000000000000000, -3.421497350147988392 ) ) ;
#8078 = EDGE_LOOP ( 'NONE', ( #4464, #11497, #13321, #4805 ) ) ;
#8079 = FACE_OUTER_BOUND ( 'NONE', #1776, .T. ) ;
#8080 =( NAMED_UNIT ( * ) SI_UNIT ( $, .STERADIAN. ) SOLID_ANGLE_UNIT ( ) );
#8081 = CARTESIAN_POINT ( 'NONE',  ( 7.248474140376191421, 0.000000000000000000, 4.439552076088042476 ) ) ;
#8082 = LINE ( 'NONE', #1956, #9460 ) ;
#8083 = ADVANCED_FACE ( 'NONE', ( #426 ), #2585, .F. ) ;
#8084 = DIRECTION ( 'NONE',  ( 0.000000000000000000, 1.000000000000000000, 0.000000000000000000 ) ) ;
#8085 = EDGE_CURVE ( 'NONE', #10517, #5245, #5693, .T. ) ;
#8086 = CARTESIAN_POINT ( 'NONE',  ( -6.017756925049793537, 3.000000000000000000, -11.52330688609026232 ) ) ;
#8087 = CARTESIAN_POINT ( 'NONE',  ( 1.580708947611199511, 0.000000000000000000, -8.351727918397596540 ) ) ;
#8088 = FACE_BOUND ( 'NONE', #3422, .T. ) ;
#8089 = CARTESIAN_POINT ( 'NONE',  ( 10.18979803820052155, 3.000000000000000000, -6.506620931068708202 ) ) ;
#8090 = ORIENTED_EDGE ( 'NONE', *, *, #6830, .F. ) ;
#8091 = ORIENTED_EDGE ( 'NONE', *, *, #7363, .T. ) ;
#8092 = ORIENTED_EDGE ( 'NONE', *, *, #1270, .T. ) ;
#8093 = VERTEX_POINT ( 'NONE', #4362 ) ;
#8094 = CARTESIAN_POINT ( 'NONE',  ( 7.499999999999999112, 3.000000000000000000, 0.000000000000000000 ) ) ;
#8095 = DIRECTION ( 'NONE',  ( 0.000000000000000000, 1.000000000000000000, 0.000000000000000000 ) ) ;
#8096 = EDGE_CURVE ( 'NONE', #5500, #12749, #11666, .T. ) ;
#8097 = ADVANCED_FACE ( 'NONE', ( #3453 ), #7662, .F. ) ;
#8098 = CYLINDRICAL_SURFACE ( 'NONE', #11727, 1.000000000000000888 ) ;
#8099 = DIRECTION ( 'NONE',  ( -1.000000000000000000, 3.469446951953610639E-15, 2.602085213965210149E-16 ) ) ;
#8100 = CARTESIAN_POINT ( 'NONE',  ( -13.49999999999999645, 0.000000000000000000, -7.049999999999998934 ) ) ;
#8101 = EDGE_CURVE ( 'NONE', #8964, #5111, #5549, .T. ) ;
#8102 = EDGE_CURVE ( 'NONE', #12066, #11098, #6434, .T. ) ;
#8103 = FACE_OUTER_BOUND ( 'NONE', #4424, .T. ) ;
#8104 = AXIS2_PLACEMENT_3D ( 'NONE', #5028, #834, #8127 ) ;
#8105 = CARTESIAN_POINT ( 'NONE',  ( 10.72973591378220704, 3.000000000000000000, -5.571433138827823761 ) ) ;
#8106 = ORIENTED_EDGE ( 'NONE', *, *, #8881, .T. ) ;
#8107 = CARTESIAN_POINT ( 'NONE',  ( 8.481367827640703183, 0.000000000000000000, 0.5624942419805130100 ) ) ;
#8108 = CARTESIAN_POINT ( 'NONE',  ( -11.48836750521728689, 3.000000000000000000, -8.430890348300561499 ) ) ;
#8109 = ORIENTED_EDGE ( 'NONE', *, *, #5146, .F. ) ;
#8110 = B_SPLINE_CURVE_WITH_KNOTS ( 'NONE', 2,
 ( #10091, #2935, #11199 ),
 .UNSPECIFIED., .F., .F.,
 ( 3, 3 ),
 ( 0.000000000000000000, 1.000000000000000000 ),
 .UNSPECIFIED. ) ;
#8111 = CARTESIAN_POINT ( 'NONE',  ( 9.593885948927676210, 0.000000000000000000, -8.504652361247169168 ) ) ;
#8112 = CARTESIAN_POINT ( 'NONE',  ( 59.20906036370105596, 32.33135765298362685, 9.098535593482273143 ) ) ;
#8113 = CARTESIAN_POINT ( 'NONE',  ( -13.49999999999999645, 3.000000000000000000, -7.049999999999998934 ) ) ;
#8114 = DIRECTION ( 'NONE',  ( 0.000000000000000000, 0.000000000000000000, -1.000000000000000000 ) ) ;
#8115 = DIRECTION ( 'NONE',  ( 0.000000000000000000, 1.000000000000000000, 0.000000000000000000 ) ) ;
#8116 = CARTESIAN_POINT ( 'NONE',  ( 3.188443874008702661, 3.000000000000000000, -12.60833581801614578 ) ) ;
#8117 = CARTESIAN_POINT ( 'NONE',  ( -11.17001009226120445, 0.000000000000000000, -6.660869730750943241 ) ) ;
#8118 = ORIENTED_EDGE ( 'NONE', *, *, #5555, .T. ) ;
#8119 = CARTESIAN_POINT ( 'NONE',  ( -7.500000000000000000, 3.000000000000000000, -1.500000000000000666 ) ) ;
#8120 = EDGE_LOOP ( 'NONE', ( #2517, #1934, #3763, #6610 ) ) ;
#8121 = ORIENTED_EDGE ( 'NONE', *, *, #7896, .F. ) ;
#8122 = CARTESIAN_POINT ( 'NONE',  ( 12.37962962962963864, 0.000000000000000000, -12.43467921358330663 ) ) ;
#8123 = AXIS2_PLACEMENT_3D ( 'NONE', #8659, #4603, #10877 ) ;
#8124 = VERTEX_POINT ( 'NONE', #307 ) ;
#8125 = ADVANCED_FACE ( 'NONE', ( #4499 ), #7745, .T. ) ;
#8126 = EDGE_LOOP ( 'NONE', ( #12939, #3935, #4099, #13355 ) ) ;
#8127 = DIRECTION ( 'NONE',  ( 0.000000000000000000, 0.000000000000000000, -1.000000000000000000 ) ) ;
#8128 = CARTESIAN_POINT ( 'NONE',  ( -0.6724118135763151871, 0.000000000000000000, -13.82336506795071784 ) ) ;
#8129 = CARTESIAN_POINT ( 'NONE',  ( -2.590203375110137873, 9.000000000000000000, 6.893050072893555758 ) ) ;
#8130 = LINE ( 'NONE', #13577, #4257 ) ;
#8131 = CARTESIAN_POINT ( 'NONE',  ( 0.7944557581062193785, 9.000000000000000000, -6.703084368289860429 ) ) ;
#8132 = VECTOR ( 'NONE', #2327, 1000.000000000000000 ) ;
#8133 = FACE_OUTER_BOUND ( 'NONE', #6833, .T. ) ;
#8134 = VERTEX_POINT ( 'NONE', #12769 ) ;
#8135 = DIRECTION ( 'NONE',  ( -0.000000000000000000, -1.000000000000000000, 0.000000000000000000 ) ) ;
#8136 = ORIENTED_EDGE ( 'NONE', *, *, #11566, .T. ) ;
#8137 = EDGE_LOOP ( 'NONE', ( #13222, #4023, #2144, #830 ) ) ;
#8138 = DIRECTION ( 'NONE',  ( 0.6291930273682727615, 0.000000000000000000, -0.7772490812546181127 ) ) ;
#8139 = EDGE_LOOP ( 'NONE', ( #5560, #11842, #6977, #8765 ) ) ;
#8140 = AXIS2_PLACEMENT_3D ( 'NONE', #7943, #10683, #9639 ) ;
#8141 = CARTESIAN_POINT ( 'NONE',  ( 8.158651161643900807, 3.000000000000000000, 8.922136023539609440 ) ) ;
#8142 = DIRECTION ( 'NONE',  ( -0.9100336346413742117, -0.000000000000000000, -0.4145344181384821858 ) ) ;
#8143 = PLANE ( 'NONE',  #2420 ) ;
#8144 = CARTESIAN_POINT ( 'NONE',  ( 3.000000000000001776, 2.000000000000000000, 10.00000000000000000 ) ) ;
#8145 = CARTESIAN_POINT ( 'NONE',  ( 3.469446951953614189E-15, 0.000000000000000000, -7.049999999999999822 ) ) ;
#8146 = CARTESIAN_POINT ( 'NONE',  ( 5.053288777954491273, 1.734723475976807094E-15, -4.475128213425755952 ) ) ;
#8147 = CARTESIAN_POINT ( 'NONE',  ( 11.90209577080759296, 3.000000000000000000, -8.180229652970856691 ) ) ;
#8148 = CARTESIAN_POINT ( 'NONE',  ( -1.119409668803374558, 0.000000000000000000, -13.50845331674225669 ) ) ;
#8149 = FACE_OUTER_BOUND ( 'NONE', #12776, .T. ) ;
#8150 = CIRCLE ( 'NONE', #1560, 14.25000000000000000 ) ;
#8151 = VECTOR ( 'NONE', #7975, 1000.000000000000000 ) ;
#8152 = ORIENTED_EDGE ( 'NONE', *, *, #12581, .T. ) ;
#8153 = ORIENTED_EDGE ( 'NONE', *, *, #10021, .F. ) ;
#8154 = EDGE_CURVE ( 'NONE', #12785, #3086, #494, .T. ) ;
#8155 = ORIENTED_EDGE ( 'NONE', *, *, #8848, .F. ) ;
#8156 = PRODUCT_RELATED_PRODUCT_CATEGORY ( 'part', '', ( #1263 ) ) ;
#8157 = EDGE_LOOP ( 'NONE', ( #5955, #12058, #8706, #9023 ) ) ;
#8158 = LINE ( 'NONE', #5060, #5787 ) ;
#8159 = CIRCLE ( 'NONE', #4642, 1.500000000000001332 ) ;
#8160 = DIRECTION ( 'NONE',  ( 0.000000000000000000, 0.000000000000000000, 1.000000000000000000 ) ) ;
#8161 = CARTESIAN_POINT ( 'NONE',  ( -5.250000000000000000, 0.000000000000000000, -26.44078293894052578 ) ) ;
#8162 = CARTESIAN_POINT ( 'NONE',  ( 6.506507307819716424, 3.000000000000000000, -10.18987059060247269 ) ) ;
#8163 = FACE_OUTER_BOUND ( 'NONE', #1853, .T. ) ;
#8164 = FACE_OUTER_BOUND ( 'NONE', #323, .T. ) ;
#8165 = EDGE_LOOP ( 'NONE', ( #13450, #11071, #6764, #877, #8402 ) ) ;
#8166 = VECTOR ( 'NONE', #12074, 1000.000000000000000 ) ;
#8167 = CARTESIAN_POINT ( 'NONE',  ( 7.363612555047485131, 0.000000000000000000, -0.02242701489043354146 ) ) ;
#8168 = EDGE_CURVE ( 'NONE', #2208, #3304, #9319, .T. ) ;
#8169 = CARTESIAN_POINT ( 'NONE',  ( -4.227250083625790467, 3.000000000000000000, -13.17831234185026013 ) ) ;
#8170 = ORIENTED_EDGE ( 'NONE', *, *, #2799, .F. ) ;
#8171 = EDGE_CURVE ( 'NONE', #13138, #7859, #12077, .T. ) ;
#8172 = EDGE_CURVE ( 'NONE', #7143, #3990, #7321, .T. ) ;
#8173 = FACE_OUTER_BOUND ( 'NONE', #11129, .T. ) ;
#8174 = AXIS2_PLACEMENT_3D ( 'NONE', #9553, #3265, #134 ) ;
#8175 = DIRECTION ( 'NONE',  ( 0.6405005040948713591, 0.000000000000000000, -0.7679577490033002718 ) ) ;
#8176 = AXIS2_PLACEMENT_3D ( 'NONE', #3673, #12241, #4719 ) ;
#8177 = CARTESIAN_POINT ( 'NONE',  ( -12.55526518755974585, 0.000000000000000000, -2.546103534247746047 ) ) ;
#8178 = CARTESIAN_POINT ( 'NONE',  ( -5.039625798601655937, 0.000000000000000000, 4.490509081392511703 ) ) ;
#8179 = CARTESIAN_POINT ( 'NONE',  ( -11.90284147956865723, 3.000000000000000000, -9.133371500908332052 ) ) ;
#8180 = CARTESIAN_POINT ( 'NONE',  ( -2.161962830978783057, 3.000000000000000000, -14.08504230442586369 ) ) ;
#8181 = CARTESIAN_POINT ( 'NONE',  ( -11.11702303352197063, 3.000000000000000000, -8.914835885878215294 ) ) ;
#8182 =( REPRESENTATION_RELATIONSHIP ('NONE','NONE', #3798, #8539 ) REPRESENTATION_RELATIONSHIP_WITH_TRANSFORMATION ( #12161 )SHAPE_REPRESENTATION_RELATIONSHIP( ) );
#8183 = ADVANCED_FACE ( 'NONE', ( #1678 ), #4904, .T. ) ;
#8184 = VERTEX_POINT ( 'NONE', #10213 ) ;
#8185 = UNCERTAINTY_MEASURE_WITH_UNIT (LENGTH_MEASURE( 1.000000000000000082E-05 ), #1954, 'distance_accuracy_value', 'NONE');
#8186 = VECTOR ( 'NONE', #8138, 1000.000000000000000 ) ;
#8187 = ORIENTED_EDGE ( 'NONE', *, *, #4597, .F. ) ;
#8188 = CARTESIAN_POINT ( 'NONE',  ( 0.4639228963249696913, 9.000000000000000000, 8.487330295579727846 ) ) ;
#8189 = CIRCLE ( 'NONE', #7971, 5.500000000000000000 ) ;
#8190 = AXIS2_PLACEMENT_3D ( 'NONE', #2834, #4699, #7926 ) ;
#8192 = ORIENTED_EDGE ( 'NONE', *, *, #9428, .F. ) ;
#8191 = B_SPLINE_CURVE_WITH_KNOTS ( 'NONE', 3,
 ( #1215, #12031, #9872, #11878 ),
 .UNSPECIFIED., .F., .F.,
 ( 4, 4 ),
 ( 0.000000000000000000, 0.8452273900860258760 ),
 .UNSPECIFIED. ) ;
#8193 = EDGE_CURVE ( 'NONE', #3554, #8734, #3716, .T. ) ;
#8194 = CARTESIAN_POINT ( 'NONE',  ( 31.00000000000000000, 0.000000000000000000, 0.000000000000000000 ) ) ;
#8195 = CARTESIAN_POINT ( 'NONE',  ( -6.017756925049793537, 0.000000000000000000, -11.52330688609026232 ) ) ;
#8196 = DIRECTION ( 'NONE',  ( 0.000000000000000000, 0.000000000000000000, -1.000000000000000000 ) ) ;
#8197 = COLOUR_RGB ( '',0.7803921568627451011, 0.7607843137254901578, 0.7411764705882353255 ) ;
#8198 = CARTESIAN_POINT ( 'NONE',  ( 20.03271148078819408, 0.000000000000000000, -5.075121771833452478 ) ) ;
#8199 = FACE_OUTER_BOUND ( 'NONE', #8635, .T. ) ;
#8200 = ORIENTED_EDGE ( 'NONE', *, *, #8696, .T. ) ;
#8201 = FACE_OUTER_BOUND ( 'NONE', #3321, .T. ) ;
#8202 = ADVANCED_FACE ( 'NONE', ( #3656, #1606, #2694 ), #3592, .T. ) ;
#8203 = ORIENTED_EDGE ( 'NONE', *, *, #6982, .T. ) ;
#8204 = EDGE_CURVE ( 'NONE', #8258, #3500, #9068, .T. ) ;
#8205 = ORIENTED_EDGE ( 'NONE', *, *, #12116, .T. ) ;
#8206 = CARTESIAN_POINT ( 'NONE',  ( 7.771282357155270937, 9.000000000000000000, -3.443424244174282833 ) ) ;
#8207 = VERTEX_POINT ( 'NONE', #8001 ) ;
#8208 = VECTOR ( 'NONE', #2775, 1000.000000000000000 ) ;
#8209 = AXIS2_PLACEMENT_3D ( 'NONE', #8700, #12854, #9735 ) ;
#8210 = VECTOR ( 'NONE', #8779, 1000.000000000000000 ) ;
#8211 = DIRECTION ( 'NONE',  ( 0.000000000000000000, 1.000000000000000000, 0.000000000000000000 ) ) ;
#8212 = FILL_AREA_STYLE_COLOUR ( '', #4065 ) ;
#8213 = LINE ( 'NONE', #2989, #3791 ) ;
#8214 = LINE ( 'NONE', #9393, #11658 ) ;
#8215 = CARTESIAN_POINT ( 'NONE',  ( 12.01285915242476499, 3.000000000000000000, -4.000000001073668265 ) ) ;
#8216 = CYLINDRICAL_SURFACE ( 'NONE', #6237, 1.500000000000000222 ) ;
#8217 = CARTESIAN_POINT ( 'NONE',  ( 0.000000000000000000, 0.000000000000000000, 0.000000000000000000 ) ) ;
#8218 = CARTESIAN_POINT ( 'NONE',  ( 31.00000000000000000, 3.000000000000000000, -1.500000000759764029 ) ) ;
#8219 = CIRCLE ( 'NONE', #11747, 3.000000000000000000 ) ;
#8220 = ORIENTED_EDGE ( 'NONE', *, *, #4305, .T. ) ;
#8221 = CARTESIAN_POINT ( 'NONE',  ( 12.25282671965375592, 3.000000000000000000, -5.797378255456012930 ) ) ;
#8222 = VECTOR ( 'NONE', #12962, 1000.000000000000000 ) ;
#8223 = ORIENTED_EDGE ( 'NONE', *, *, #1631, .F. ) ;
#8224 = ORIENTED_EDGE ( 'NONE', *, *, #8932, .F. ) ;
#8225 = ORIENTED_EDGE ( 'NONE', *, *, #10901, .F. ) ;
#8226 = VERTEX_POINT ( 'NONE', #5798 ) ;
#8227 = DIRECTION ( 'NONE',  ( 0.000000000000000000, 1.000000000000000000, 0.000000000000000000 ) ) ;
#8228 = AXIS2_PLACEMENT_3D ( 'NONE', #10596, #1157, #5355 ) ;
#8229 = CIRCLE ( 'NONE', #11989, 2.750000000000002665 ) ;
#8230 = FACE_OUTER_BOUND ( 'NONE', #5559, .T. ) ;
#8231 = B_SPLINE_CURVE_WITH_KNOTS ( 'NONE', 2,
 ( #10320, #8179, #6254 ),
 .UNSPECIFIED., .F., .F.,
 ( 3, 3 ),
 ( 0.000000000000000000, 1.000000000000000000 ),
 .UNSPECIFIED. ) ;
#8232 = CARTESIAN_POINT ( 'NONE',  ( 10.72973591378220704, 0.000000000000000000, -5.571433138827823761 ) ) ;
#8233 = CARTESIAN_POINT ( 'NONE',  ( 0.000000000000000000, 2.900000000000000355, 0.000000000000000000 ) ) ;
#8234 = DIRECTION ( 'NONE',  ( -0.000000000000000000, -1.000000000000000000, -0.000000000000000000 ) ) ;
#8235 = EDGE_CURVE ( 'NONE', #2261, #3498, #9946, .T. ) ;
#8236 = CARTESIAN_POINT ( 'NONE',  ( 0.000000000000000000, 0.000000000000000000, 0.000000000000000000 ) ) ;
#8237 = AXIS2_PLACEMENT_3D ( 'NONE', #1411, #584, #4779 ) ;
#8238 = DIRECTION ( 'NONE',  ( -0.000000000000000000, -1.000000000000000000, -0.000000000000000000 ) ) ;
#8239 = AXIS2_PLACEMENT_3D ( 'NONE', #9399, #4094, #11532 ) ;
#8240 = VERTEX_POINT ( 'NONE', #6761 ) ;
#8241 = LINE ( 'NONE', #3901, #7085 ) ;
#8242 = CIRCLE ( 'NONE', #11549, 12.08999999999737440 ) ;
#8243 = LINE ( 'NONE', #5214, #10848 ) ;
#8244 = EDGE_LOOP ( 'NONE', ( #2031, #9729, #6426, #10950 ) ) ;
#8245 = B_SPLINE_CURVE_WITH_KNOTS ( 'NONE', 3,
 ( #1000, #1196, #3833, #7400 ),
 .UNSPECIFIED., .F., .F.,
 ( 4, 4 ),
 ( 0.000000000000000000, 0.8452273900860258760 ),
 .UNSPECIFIED. ) ;
#8246 = FACE_OUTER_BOUND ( 'NONE', #5024, .T. ) ;
#8247 = APPLICATION_PROTOCOL_DEFINITION ( 'draft international standard', 'automotive_design', 1998, #10114 ) ;
#8248 = CIRCLE ( 'NONE', #4078, 6.749999999999999112 ) ;
#8249 = EDGE_CURVE ( 'NONE', #1536, #7207, #11782, .T. ) ;
#8250 = DIRECTION ( 'NONE',  ( 0.000000000000000000, 0.000000000000000000, 1.000000000000000000 ) ) ;
#8251 = DIRECTION ( 'NONE',  ( 0.000000000000000000, 1.000000000000000000, -0.000000000000000000 ) ) ;
#8252 = EDGE_CURVE ( 'NONE', #9891, #1728, #4014, .T. ) ;
#8253 = LINE ( 'NONE', #7227, #4280 ) ;
#8254 = EDGE_CURVE ( 'NONE', #11718, #8926, #8645, .T. ) ;
#8255 = CYLINDRICAL_SURFACE ( 'NONE', #2541, 1.000000000000000888 ) ;
#8256 = CARTESIAN_POINT ( 'NONE',  ( 5.517918333394296049, 0.000000000000000000, 4.875228826198821253 ) ) ;
#8257 = EDGE_CURVE ( 'NONE', #2790, #76, #2407, .T. ) ;
#8258 = VERTEX_POINT ( 'NONE', #5720 ) ;
#8259 = STYLED_ITEM ( 'NONE', ( #7499 ), #7847 ) ;
#8260 = VERTEX_POINT ( 'NONE', #498 ) ;
#8261 = CARTESIAN_POINT ( 'NONE',  ( 0.000000000000000000, 0.000000000000000000, 0.000000000000000000 ) ) ;
#8262 = EDGE_LOOP ( 'NONE', ( #7739, #12425, #3838, #11921 ) ) ;
#8263 = DIRECTION ( 'NONE',  ( 0.000000000000000000, 0.000000000000000000, 1.000000000000000000 ) ) ;
#8264 = CARTESIAN_POINT ( 'NONE',  ( -14.82803603298498629, 3.000000000000000000, 2.264806262023049577 ) ) ;
#8265 = EDGE_CURVE ( 'NONE', #710, #3254, #706, .T. ) ;
#8266 = CARTESIAN_POINT ( 'NONE',  ( 0.000000000000000000, 1.000000000000000000, 0.000000000000000000 ) ) ;
#8267 = PRODUCT_DEFINITION_FORMATION_WITH_SPECIFIED_SOURCE ( 'ANY', '', #5568, .NOT_KNOWN. ) ;
#8268 = FACE_OUTER_BOUND ( 'NONE', #11721, .T. ) ;
#8269 = DIRECTION ( 'NONE',  ( 0.000000000000000000, 1.000000000000000000, 0.000000000000000000 ) ) ;
#8270 = CARTESIAN_POINT ( 'NONE',  ( 1.958311002203130480, 3.000000000000000000, -14.87484884897977366 ) ) ;
#8271 = ORIENTED_EDGE ( 'NONE', *, *, #1033, .T. ) ;
#8272 = EDGE_CURVE ( 'NONE', #10261, #2378, #10841, .T. ) ;
#8273 = DIRECTION ( 'NONE',  ( 0.000000000000000000, 0.000000000000000000, -1.000000000000000000 ) ) ;
#8274 = EDGE_CURVE ( 'NONE', #7331, #11192, #4773, .T. ) ;
#8275 = ORIENTED_EDGE ( 'NONE', *, *, #12334, .T. ) ;
#8276 = ORIENTED_EDGE ( 'NONE', *, *, #10057, .T. ) ;
#8277 = CARTESIAN_POINT ( 'NONE',  ( 31.00000000000000000, 3.000000000000000000, 0.000000000000000000 ) ) ;
#8278 = VERTEX_POINT ( 'NONE', #2011 ) ;
#8279 = FACE_OUTER_BOUND ( 'NONE', #9743, .T. ) ;
#8280 = DIRECTION ( 'NONE',  ( 0.000000000000000000, 1.000000000000000000, 0.000000000000000000 ) ) ;
#8281 = CARTESIAN_POINT ( 'NONE',  ( 6.506620931068707314, 3.000000000000000000, 10.18979803820051622 ) ) ;
#8282 = DIRECTION ( 'NONE',  ( -0.000000000000000000, -1.000000000000000000, -0.000000000000000000 ) ) ;
#8283 = CARTESIAN_POINT ( 'NONE',  ( -5.708888906988910605, 3.000000000000000000, 11.46847481510586597 ) ) ;
#8284 = FACE_OUTER_BOUND ( 'NONE', #1628, .T. ) ;
#8285 = CARTESIAN_POINT ( 'NONE',  ( -7.668956737359326148, 0.000000000000000000, -2.066866683227997825 ) ) ;
#8286 = LINE ( 'NONE', #9183, #4649 ) ;
#8287 = CARTESIAN_POINT ( 'NONE',  ( 6.079397157347990799, -1.694065894508600678E-18, 5.110946565852551693 ) ) ;
#8288 = B_SPLINE_CURVE_WITH_KNOTS ( 'NONE', 3,
 ( #8281, #8408, #13531, #5116 ),
 .UNSPECIFIED., .F., .F.,
 ( 4, 4 ),
 ( 0.1547128134717859205, 1.000000000000000000 ),
 .UNSPECIFIED. ) ;
#8289 = EDGE_LOOP ( 'NONE', ( #1713, #11224, #7369, #1983 ) ) ;
#8290 = CYLINDRICAL_SURFACE ( 'NONE', #4238, 1.500000000000000222 ) ;
#8291 = ORIENTED_EDGE ( 'NONE', *, *, #5806, .T. ) ;
#8292 = ORIENTED_EDGE ( 'NONE', *, *, #3468, .F. ) ;
#8293 = ORIENTED_EDGE ( 'NONE', *, *, #2334, .F. ) ;
#8294 = ORIENTED_EDGE ( 'NONE', *, *, #3782, .F. ) ;
#8295 = DIRECTION ( 'NONE',  ( 0.000000000000000000, 0.000000000000000000, 1.000000000000000000 ) ) ;
#8296 = CARTESIAN_POINT ( 'NONE',  ( 11.11702303352194043, 3.000000000000000000, -8.914835885878249044 ) ) ;
#8297 = EDGE_CURVE ( 'NONE', #3277, #12193, #12612, .T. ) ;
#8298 = EDGE_CURVE ( 'NONE', #1592, #8260, #12501, .T. ) ;
#8299 = CARTESIAN_POINT ( 'NONE',  ( 30.66173999750687784, 0.000000000000000000, 0.01003121477750366919 ) ) ;
#8300 = DIRECTION ( 'NONE',  ( -0.000000000000000000, -1.000000000000000000, -0.000000000000000000 ) ) ;
#8301 = CARTESIAN_POINT ( 'NONE',  ( 12.00000000000001243, 5.000000000000000000, 7.000000000000000888 ) ) ;
#8302 = CARTESIAN_POINT ( 'NONE',  ( 40.92955321648837241, 3.000000000000000000, -6.070049343411170639 ) ) ;
#8303 = ORIENTED_EDGE ( 'NONE', *, *, #8959, .F. ) ;
#8304 = CARTESIAN_POINT ( 'NONE',  ( -1.604252589105048976, 0.000000000000000000, -8.347237484961699039 ) ) ;
#8305 = CARTESIAN_POINT ( 'NONE',  ( 3.850308450823737516, 9.000000000000000000, 5.544152309732777617 ) ) ;
#8307 = VERTEX_POINT ( 'NONE', #6206 ) ;
#8306 = B_SPLINE_CURVE_WITH_KNOTS ( 'NONE', 3,
 ( #6746, #10949, #12606, #6190 ),
 .UNSPECIFIED., .F., .F.,
 ( 4, 4 ),
 ( 0.000000000000000000, 0.5855695330273008592 ),
 .UNSPECIFIED. ) ;
#8308 = DIRECTION ( 'NONE',  ( -0.000000000000000000, -1.000000000000000000, -0.000000000000000000 ) ) ;
#8309 = DIRECTION ( 'NONE',  ( 0.000000000000000000, 0.000000000000000000, 1.000000000000000000 ) ) ;
#8310 = PRODUCT_CONTEXT ( 'NONE', #4935, 'mechanical' ) ;
#8311 = CARTESIAN_POINT ( 'NONE',  ( 0.000000000000000000, 0.000000000000000000, 0.000000000000000000 ) ) ;
#8312 = CARTESIAN_POINT ( 'NONE',  ( 10.25006213149504752, 3.000000000000000000, -9.299128225235653744 ) ) ;
#8313 = LINE ( 'NONE', #5085, #2957 ) ;
#8314 = CARTESIAN_POINT ( 'NONE',  ( -7.780961115628980629, 0.000000000000000000, -3.421497350147988392 ) ) ;
#8315 = FACE_OUTER_BOUND ( 'NONE', #11428, .T. ) ;
#8316 = EDGE_LOOP ( 'NONE', ( #8486, #4869, #12720, #10886 ) ) ;
#8317 = ORIENTED_EDGE ( 'NONE', *, *, #10459, .F. ) ;
#8318 = CARTESIAN_POINT ( 'NONE',  ( 5.967832595844252630, 0.000000000000000000, -3.153961652902406154 ) ) ;
#8319 = EDGE_CURVE ( 'NONE', #8184, #1339, #8843, .T. ) ;
#8320 = VERTEX_POINT ( 'NONE', #2904 ) ;
#8321 = DIRECTION ( 'NONE',  ( 0.000000000000000000, 0.000000000000000000, 1.000000000000000000 ) ) ;
#8322 = SURFACE_STYLE_USAGE ( .BOTH. , #10680 ) ;
#8323 = DIRECTION ( 'NONE',  ( 0.000000000000000000, 1.000000000000000000, 0.000000000000000000 ) ) ;
#8324 = FILL_AREA_STYLE_COLOUR ( '', #10580 ) ;
#8325 = DIRECTION ( 'NONE',  ( -0.000000000000000000, -1.000000000000000000, -0.000000000000000000 ) ) ;
#8326 = CARTESIAN_POINT ( 'NONE',  ( 8.795158114916441505, 0.000000000000000000, -9.573149624528689117 ) ) ;
#8327 = CARTESIAN_POINT ( 'NONE',  ( 13.40069634612381044, 3.000000000000000000, 2.546644602219900300 ) ) ;
#8328 = ORIENTED_EDGE ( 'NONE', *, *, #2363, .F. ) ;
#8329 = CARTESIAN_POINT ( 'NONE',  ( -11.11702303352192445, 0.000000000000000000, 8.914835885878272137 ) ) ;
#8330 = ORIENTED_EDGE ( 'NONE', *, *, #4202, .F. ) ;
#8331 = B_SPLINE_CURVE_WITH_KNOTS ( 'NONE', 3,
 ( #3652, #7852, #633, #1672 ),
 .UNSPECIFIED., .F., .F.,
 ( 4, 4 ),
 ( 0.000000000000000000, 0.8724294488011758997 ),
 .UNSPECIFIED. ) ;
#8332 = EDGE_LOOP ( 'NONE', ( #608, #3266, #13100, #12879 ) ) ;
#8333 = CARTESIAN_POINT ( 'NONE',  ( -10.15083332828461771, 0.000000000000000000, -29.86148447151320795 ) ) ;
#8334 = EDGE_CURVE ( 'NONE', #3990, #6631, #9233, .T. ) ;
#8335 = VERTEX_POINT ( 'NONE', #4975 ) ;
#8336 = DIRECTION ( 'NONE',  ( 0.000000000000000000, 0.000000000000000000, -1.000000000000000000 ) ) ;
#8337 = EDGE_CURVE ( 'NONE', #6519, #6591, #9538, .T. ) ;
#8338 = DIRECTION ( 'NONE',  ( -0.000000000000000000, -1.000000000000000000, -0.000000000000000000 ) ) ;
#8339 = EDGE_CURVE ( 'NONE', #11537, #313, #7548, .T. ) ;
#8340 = DIRECTION ( 'NONE',  ( -0.000000000000000000, -1.000000000000000000, 0.000000000000000000 ) ) ;
#8341 = FACE_OUTER_BOUND ( 'NONE', #12472, .T. ) ;
#8342 = AXIS2_PLACEMENT_3D ( 'NONE', #547, #8861, #12885 ) ;
#8343 = CARTESIAN_POINT ( 'NONE',  ( 2.999999999999995559, 2.000000000000000000, -10.00000000000000355 ) ) ;
#8344 = DIRECTION ( 'NONE',  ( -0.000000000000000000, -1.000000000000000000, -0.000000000000000000 ) ) ;
#8345 = CARTESIAN_POINT ( 'NONE',  ( 10.97318381393774089, 0.000000000000000000, -6.970598036433387712 ) ) ;
#8346 = FACE_OUTER_BOUND ( 'NONE', #6613, .T. ) ;
#8347 = VERTEX_POINT ( 'NONE', #13520 ) ;
#8348 = DIRECTION ( 'NONE',  ( 0.000000000000000000, 1.000000000000000000, -0.000000000000000000 ) ) ;
#8349 = EDGE_LOOP ( 'NONE', ( #1730, #4154, #10614, #1947 ) ) ;
#8350 = VERTEX_POINT ( 'NONE', #12362 ) ;
#8351 = CIRCLE ( 'NONE', #13195, 14.25000000000000178 ) ;
#8352 = EDGE_CURVE ( 'NONE', #12329, #5918, #11301, .T. ) ;
#8353 = VECTOR ( 'NONE', #12567, 1000.000000000000000 ) ;
#8354 = VERTEX_POINT ( 'NONE', #910 ) ;
#8355 = VERTEX_POINT ( 'NONE', #9439 ) ;
#8356 = CARTESIAN_POINT ( 'NONE',  ( -1.557181465540221188, 3.000000000000000000, 14.16466328168015743 ) ) ;
#8357 = EDGE_CURVE ( 'NONE', #2239, #7175, #9384, .T. ) ;
#8358 = CARTESIAN_POINT ( 'NONE',  ( 12.48730470360076161, 0.000000000000000000, -6.329867395090054139 ) ) ;
#8359 = CIRCLE ( 'NONE', #10126, 14.25000000000000000 ) ;
#8360 =( REPRESENTATION_RELATIONSHIP ('NONE','NONE', #3798, #7939 ) REPRESENTATION_RELATIONSHIP_WITH_TRANSFORMATION ( #13048 )SHAPE_REPRESENTATION_RELATIONSHIP( ) );
#8361 = FACE_OUTER_BOUND ( 'NONE', #11503, .T. ) ;
#8362 = CARTESIAN_POINT ( 'NONE',  ( 7.065816209474156118, 0.000000000000000000, -10.69794375946289833 ) ) ;
#8363 = VECTOR ( 'NONE', #5494, 1000.000000000000000 ) ;
#8364 = B_SPLINE_CURVE_WITH_KNOTS ( 'NONE', 3,
 ( #2601, #5696, #1299, #7894 ),
 .UNSPECIFIED., .F., .F.,
 ( 4, 4 ),
 ( 0.000000000000000000, 0.8452273900860258760 ),
 .UNSPECIFIED. ) ;
#8365 = VERTEX_POINT ( 'NONE', #6078 ) ;
#8366 = VERTEX_POINT ( 'NONE', #979 ) ;
#8367 = DIRECTION ( 'NONE',  ( 0.000000000000000000, 0.000000000000000000, -1.000000000000000000 ) ) ;
#8368 = EDGE_CURVE ( 'NONE', #833, #1513, #7335, .T. ) ;
#8369 = DIRECTION ( 'NONE',  ( 0.000000000000000000, 0.000000000000000000, -1.000000000000000000 ) ) ;
#8370 = AXIS2_PLACEMENT_3D ( 'NONE', #7821, #2249, #3416 ) ;
#8371 = ORIENTED_EDGE ( 'NONE', *, *, #9345, .T. ) ;
#8372 = CYLINDRICAL_SURFACE ( 'NONE', #962, 1.500000000000001332 ) ;
#8373 = CARTESIAN_POINT ( 'NONE',  ( 41.67875868938293138, 3.000000000000000000, -6.066649533482935119 ) ) ;
#8374 = DIRECTION ( 'NONE',  ( 0.5581732849759741821, 2.202450710935965086E-26, 0.8297244024006588115 ) ) ;
#8375 = CARTESIAN_POINT ( 'NONE',  ( 19.65244806805498357, 0.000000000000000000, -6.000000000000000000 ) ) ;
#8376 = SHAPE_REPRESENTATION ( 'base-gear', ( #10007 ), #6493 ) ;
#8377 = FACE_OUTER_BOUND ( 'NONE', #559, .T. ) ;
#8378 = CIRCLE ( 'NONE', #5295, 1.500000000000000222 ) ;
#8379 = FACE_OUTER_BOUND ( 'NONE', #1029, .T. ) ;
#8380 = DIRECTION ( 'NONE',  ( -0.000000000000000000, -1.000000000000000000, -0.000000000000000000 ) ) ;
#8381 = ORIENTED_EDGE ( 'NONE', *, *, #271, .T. ) ;
#8382 = ORIENTED_EDGE ( 'NONE', *, *, #8508, .F. ) ;
#8383 = DIRECTION ( 'NONE',  ( 0.000000000000000000, 0.000000000000000000, 1.000000000000000000 ) ) ;
#8384 = VERTEX_POINT ( 'NONE', #8329 ) ;
#8385 = EDGE_CURVE ( 'NONE', #13453, #11685, #12565, .T. ) ;
#8386 = AXIS2_PLACEMENT_3D ( 'NONE', #2361, #4293, #5590 ) ;
#8387 = CARTESIAN_POINT ( 'NONE',  ( -7.235926821844434365, 9.000000000000000000, 4.459973433655444630 ) ) ;
#8388 = B_SPLINE_SURFACE_WITH_KNOTS ( 'NONE', 3, 1, ( 
 ( #8131, #11239 ),
 ( #5237, #4135 ),
 ( #3034, #10210 ),
 ( #1808, #2974 ) ),
 .UNSPECIFIED., .F., .F., .F.,
 ( 4, 4 ),
 ( 2, 2 ),
 ( 0.000000000000000000, 0.8724294488011757887 ),
 ( 0.000000000000000000, 1.000000000000000000 ),
 .UNSPECIFIED. ) ;
#8389 = CARTESIAN_POINT ( 'NONE',  ( 0.000000000000000000, 0.000000000000000000, 5.000000000000000000 ) ) ;
#8390 = CARTESIAN_POINT ( 'NONE',  ( 4.227250083625740729, 0.000000000000000000, -13.17831234185050526 ) ) ;
#8391 = CARTESIAN_POINT ( 'NONE',  ( 0.5501230721522984979, 0.000000000000000000, -12.98835496148321766 ) ) ;
#8392 = CARTESIAN_POINT ( 'NONE',  ( 23.99887587215152607, 3.000000000000000000, 4.000000000000000000 ) ) ;
#8393 = DIRECTION ( 'NONE',  ( 0.000000000000000000, 0.000000000000000000, 1.000000000000000000 ) ) ;
#8394 = EDGE_CURVE ( 'NONE', #11839, #2012, #1175, .T. ) ;
#8395 = EDGE_LOOP ( 'NONE', ( #626, #4596, #6546, #9066 ) ) ;
#8396 = CARTESIAN_POINT ( 'NONE',  ( -2.632142621505047408, 9.000000000000000000, -6.877144614729746586 ) ) ;
#8397 = AXIS2_PLACEMENT_3D ( 'NONE', #4825, #2492, #13311 ) ;
#8398 = AXIS2_PLACEMENT_3D ( 'NONE', #1581, #13088, #2548 ) ;
#8399 = ORIENTED_EDGE ( 'NONE', *, *, #3385, .F. ) ;
#8400 = ORIENTED_EDGE ( 'NONE', *, *, #9345, .F. ) ;
#8401 = DIRECTION ( 'NONE',  ( -3.469446951953610639E-15, -1.000000000000000000, -2.891205793294675861E-16 ) ) ;
#8402 = ORIENTED_EDGE ( 'NONE', *, *, #6450, .T. ) ;
#8403 = CARTESIAN_POINT ( 'NONE',  ( 0.000000000000000000, 1.000000000000000000, -1.500000000000000222 ) ) ;
#8404 = AXIS2_PLACEMENT_3D ( 'NONE', #99, #7452, #164 ) ;
#8405 = CARTESIAN_POINT ( 'NONE',  ( 22.00000000000000000, 3.000000000000000000, 0.000000000000000000 ) ) ;
#8406 = AXIS2_PLACEMENT_3D ( 'NONE', #1805, #3031, #11434 ) ;
#8407 = VECTOR ( 'NONE', #13399, 1000.000000000000000 ) ;
#8408 = CARTESIAN_POINT ( 'NONE',  ( 7.077546079049268357, 3.000000000000000000, 10.67828022838850544 ) ) ;
#8409 = CARTESIAN_POINT ( 'NONE',  ( 1.959434878635765477E-16, 2.900000000000000355, -1.600000000000000311 ) ) ;
#8410 = CARTESIAN_POINT ( 'NONE',  ( 23.99887587215152251, 0.000000000000000000, 5.000000000000000888 ) ) ;
#8411 = CARTESIAN_POINT ( 'NONE',  ( -14.87484884897978077, 0.000000000000000000, -1.958311002203079187 ) ) ;
#8412 = B_SPLINE_SURFACE_WITH_KNOTS ( 'NONE', 3, 1, ( 
 ( #4512, #3670 ),
 ( #5608, #8906 ),
 ( #12029, #1272 ),
 ( #4640, #4575 ) ),
 .UNSPECIFIED., .F., .F., .F.,
 ( 4, 4 ),
 ( 2, 2 ),
 ( 0.3636321741318673806, 0.3930502511895355711 ),
 ( 0.000000000000000000, 1.000000000000000000 ),
 .UNSPECIFIED. ) ;
#8413 = ADVANCED_FACE ( 'NONE', ( #12557 ), #7419, .T. ) ;
#8414 = CARTESIAN_POINT ( 'NONE',  ( -6.506620931068619385, 3.000000000000000000, -10.18979803820057306 ) ) ;
#8415 = PLANE ( 'NONE',  #8239 ) ;
#8416 = ADVANCED_FACE ( 'NONE', ( #6274 ), #3173, .F. ) ;
#8417 = ORIENTED_EDGE ( 'NONE', *, *, #1455, .F. ) ;
#8418 = CARTESIAN_POINT ( 'NONE',  ( 4.577511697546072789, 0.000000000000000000, 12.75843939030335505 ) ) ;
#8419 = ORIENTED_EDGE ( 'NONE', *, *, #11688, .T. ) ;
#8420 = CIRCLE ( 'NONE', #9951, 3.100000000000000533 ) ;
#8421 = VERTEX_POINT ( 'NONE', #4000 ) ;
#8422 = EDGE_CURVE ( 'NONE', #12500, #5440, #11318, .T. ) ;
#8423 = ORIENTED_EDGE ( 'NONE', *, *, #1969, .F. ) ;
#8424 = ORIENTED_EDGE ( 'NONE', *, *, #4323, .F. ) ;
#8425 = DIRECTION ( 'NONE',  ( 0.000000000000000000, 1.000000000000000000, 0.000000000000000000 ) ) ;
#8426 = DIRECTION ( 'NONE',  ( 0.000000000000000000, 1.000000000000000000, 0.000000000000000000 ) ) ;
#8427 = AXIS2_PLACEMENT_3D ( 'NONE', #6520, #6651, #11760 ) ;
#8428 = CARTESIAN_POINT ( 'NONE',  ( 9.250000000000003553, 2.750000000000000888, -10.00000000000000178 ) ) ;
#8429 = AXIS2_PLACEMENT_3D ( 'NONE', #9181, #10977, #1547 ) ;
#8430 = VECTOR ( 'NONE', #1158, 1000.000000000000000 ) ;
#8431 = ADVANCED_FACE ( 'NONE', ( #8201 ), #12436, .F. ) ;
#8432 = DIRECTION ( 'NONE',  ( 0.000000000000000000, 0.000000000000000000, -1.000000000000000000 ) ) ;
#8433 = CARTESIAN_POINT ( 'NONE',  ( 3.893011711613070691, 3.000000000000000000, -12.40340517008307231 ) ) ;
#8434 = ORIENTED_EDGE ( 'NONE', *, *, #279, .F. ) ;
#8435 = ORIENTED_EDGE ( 'NONE', *, *, #13185, .T. ) ;
#8436 = EDGE_CURVE ( 'NONE', #4189, #6233, #1307, .T. ) ;
#8437 = CARTESIAN_POINT ( 'NONE',  ( 10.34346111134700585, 0.000000000000000000, 8.760376775873716326 ) ) ;
#8438 = AXIS2_PLACEMENT_3D ( 'NONE', #4592, #8777, #5836 ) ;
#8439 = CIRCLE ( 'NONE', #529, 8.500000000000000000 ) ;
#8440 = MANIFOLD_SOLID_BREP ( 'Boss-Extrude1', #12598 ) ;
#8441 = AXIS2_PLACEMENT_3D ( 'NONE', #12507, #8211, #11179 ) ;
#8442 = ORIENTED_EDGE ( 'NONE', *, *, #9053, .F. ) ;
#8443 = CARTESIAN_POINT ( 'NONE',  ( -4.679611352264966051, 9.000000000000000000, -6.417326716594978997 ) ) ;
#8444 = CYLINDRICAL_SURFACE ( 'NONE', #6147, 1.499999999686092877 ) ;
#8445 = DIRECTION ( 'NONE',  ( 0.000000000000000000, 0.000000000000000000, 1.000000000000000000 ) ) ;
#8446 = CARTESIAN_POINT ( 'NONE',  ( -20.56403552112892896, 0.000000000000000000, -16.70078978407140013 ) ) ;
#8447 = DIRECTION ( 'NONE',  ( 0.000000000000000000, 0.000000000000000000, 1.000000000000000000 ) ) ;
#8448 = EDGE_CURVE ( 'NONE', #13005, #12082, #6334, .T. ) ;
#8449 = CARTESIAN_POINT ( 'NONE',  ( -13.97385902380755240, 0.000000000000000000, -5.452638258930474713 ) ) ;
#8450 = AXIS2_PLACEMENT_3D ( 'NONE', #2391, #8716, #3220 ) ;
#8451 = CARTESIAN_POINT ( 'NONE',  ( -5.731782959214987372, 3.000000000000000000, -11.46814821560793618 ) ) ;
#8452 = VECTOR ( 'NONE', #7254, 1000.000000000000227 ) ;
#8453 = FILL_AREA_STYLE ('',( #6383 ) ) ;
#8454 = VERTEX_POINT ( 'NONE', #4480 ) ;
#8455 = ORIENTED_EDGE ( 'NONE', *, *, #11230, .F. ) ;
#8456 = VERTEX_POINT ( 'NONE', #1246 ) ;
#8457 = LINE ( 'NONE', #10474, #3789 ) ;
#8458 = ORIENTED_EDGE ( 'NONE', *, *, #10386, .F. ) ;
#8459 = VECTOR ( 'NONE', #7319, 1000.000000000000000 ) ;
#8460 = FACE_BOUND ( 'NONE', #13581, .T. ) ;
#8461 = SHAPE_REPRESENTATION ( 'pin', ( #10007 ), #5191 ) ;
#8462 = DIRECTION ( 'NONE',  ( -0.000000000000000000, -1.000000000000000000, -0.000000000000000000 ) ) ;
#8463 = EDGE_CURVE ( 'NONE', #12082, #3918, #5375, .T. ) ;
#8464 = LINE ( 'NONE', #12688, #12775 ) ;
#8465 = EDGE_CURVE ( 'NONE', #1662, #8736, #12819, .T. ) ;
#8466 = DIRECTION ( 'NONE',  ( 0.000000000000000000, -0.000000000000000000, -1.000000000000000000 ) ) ;
#8467 = DIRECTION ( 'NONE',  ( -0.000000000000000000, -1.000000000000000000, -0.000000000000000000 ) ) ;
#8468 = DIRECTION ( 'NONE',  ( 0.000000000000000000, 1.000000000000000000, 0.000000000000000000 ) ) ;
#8469 = ORIENTED_EDGE ( 'NONE', *, *, #736, .F. ) ;
#8470 = CARTESIAN_POINT ( 'NONE',  ( -8.369528376005813897, 9.000000000000000000, 1.483574994138650460 ) ) ;
#8471 = ORIENTED_EDGE ( 'NONE', *, *, #6514, .T. ) ;
#8472 = AXIS2_PLACEMENT_3D ( 'NONE', #8576, #3349, #5554 ) ;
#8473 = EDGE_LOOP ( 'NONE', ( #5728, #11029, #9913, #11091 ) ) ;
#8474 = ORIENTED_EDGE ( 'NONE', *, *, #11541, .F. ) ;
#8475 = CARTESIAN_POINT ( 'NONE',  ( -8.504652361247167391, 0.000000000000000000, -9.593885948927674434 ) ) ;
#8476 = ORIENTED_EDGE ( 'NONE', *, *, #6702, .T. ) ;
#8477 = DIRECTION ( 'NONE',  ( 0.000000000000000000, 1.000000000000000000, -0.000000000000000000 ) ) ;
#8478 = EDGE_CURVE ( 'NONE', #6406, #5427, #6349, .T. ) ;
#8479 = CARTESIAN_POINT ( 'NONE',  ( 9.573149624528804580, 3.000000000000000000, -8.795158114916638681 ) ) ;
#8480 = DIRECTION ( 'NONE',  ( 0.000000000000000000, 0.000000000000000000, -1.000000000000000000 ) ) ;
#8481 = CARTESIAN_POINT ( 'NONE',  ( -9.133371500908470608, 3.000000000000000000, -11.90284147956855065 ) ) ;
#8482 = FACE_OUTER_BOUND ( 'NONE', #1699, .T. ) ;
#8483 = DIRECTION ( 'NONE',  ( 0.000000000000000000, 1.000000000000000000, 0.000000000000000000 ) ) ;
#8484 = CARTESIAN_POINT ( 'NONE',  ( -10.72973591378220348, 0.000000000000000000, 5.571433138827830867 ) ) ;
#8485 = CARTESIAN_POINT ( 'NONE',  ( -2.604531154829235362, 0.000000000000000000, -11.80612203322752585 ) ) ;
#8486 = ORIENTED_EDGE ( 'NONE', *, *, #10686, .F. ) ;
#8487 = DIRECTION ( 'NONE',  ( -0.000000000000000000, -1.000000000000000000, -0.000000000000000000 ) ) ;
#8488 = ORIENTED_EDGE ( 'NONE', *, *, #11734, .F. ) ;
#8489 = ORIENTED_EDGE ( 'NONE', *, *, #7504, .T. ) ;
#8490 = ORIENTED_EDGE ( 'NONE', *, *, #5171, .F. ) ;
#8491 = EDGE_CURVE ( 'NONE', #4274, #4058, #10747, .T. ) ;
#8492 = CARTESIAN_POINT ( 'NONE',  ( -12.98835496148299207, 3.000000000000000000, 0.5501230721524459355 ) ) ;
#8493 = PRODUCT_RELATED_PRODUCT_CATEGORY ( 'part', '', ( #10857 ) ) ;
#8494 = FACE_OUTER_BOUND ( 'NONE', #5205, .T. ) ;
#8495 = DIRECTION ( 'NONE',  ( 0.000000000000000000, 0.000000000000000000, -1.000000000000000000 ) ) ;
#8496 = DIRECTION ( 'NONE',  ( -0.000000000000000000, -1.000000000000000000, -0.000000000000000000 ) ) ;
#8497 = DIRECTION ( 'NONE',  ( 1.000000000000000000, 0.000000000000000000, 0.000000000000000000 ) ) ;
#8498 = CARTESIAN_POINT ( 'NONE',  ( 3.893011711613070691, 0.000000000000000000, -12.40340517008307231 ) ) ;
#8499 = VERTEX_POINT ( 'NONE', #8735 ) ;
#8500 = ORIENTED_EDGE ( 'NONE', *, *, #4550, .F. ) ;
#8501 = CARTESIAN_POINT ( 'NONE',  ( 4.355042381134428098, 9.000000000000000000, 7.299562031966232212 ) ) ;
#8502 = B_SPLINE_SURFACE_WITH_KNOTS ( 'NONE', 3, 1, ( 
 ( #4634, #4571 ),
 ( #13177, #7668 ),
 ( #3600, #7804 ),
 ( #5604, #5733 ) ),
 .UNSPECIFIED., .F., .F., .F.,
 ( 4, 4 ),
 ( 2, 2 ),
 ( 0.000000000000000000, 0.8452273900860258760 ),
 ( 0.000000000000000000, 1.000000000000000000 ),
 .UNSPECIFIED. ) ;
#8503 = EDGE_CURVE ( 'NONE', #11589, #1091, #13054, .T. ) ;
#8504 = EDGE_CURVE ( 'NONE', #11304, #9891, #931, .T. ) ;
#8505 = ORIENTED_EDGE ( 'NONE', *, *, #9726, .T. ) ;
#8506 = CARTESIAN_POINT ( 'NONE',  ( -12.56843238770841786, 3.000000000000000000, 3.367671042046304741 ) ) ;
#8507 = LINE ( 'NONE', #1081, #11431 ) ;
#8508 = EDGE_CURVE ( 'NONE', #11517, #6431, #89, .T. ) ;
#8509 = EDGE_CURVE ( 'NONE', #7795, #8800, #7581, .T. ) ;
#8510 = CARTESIAN_POINT ( 'NONE',  ( -3.893011711613112880, 0.000000000000000000, -12.40340517008282717 ) ) ;
#8511 = CARTESIAN_POINT ( 'NONE',  ( 4.690415759823430619, 2.900000000000000355, -4.500000000000000888 ) ) ;
#8512 = FACE_OUTER_BOUND ( 'NONE', #5151, .T. ) ;
#8513 = FACE_OUTER_BOUND ( 'NONE', #7716, .T. ) ;
#8514 = CARTESIAN_POINT ( 'NONE',  ( 5.452638258930520010, 0.000000000000000000, -13.97385902380752754 ) ) ;
#8515 = EDGE_LOOP ( 'NONE', ( #328, #7494, #5347, #7298 ) ) ;
#8516 = ORIENTED_EDGE ( 'NONE', *, *, #10649, .F. ) ;
#8517 = EDGE_LOOP ( 'NONE', ( #12662, #12696, #2571, #893 ) ) ;
#8518 = CARTESIAN_POINT ( 'NONE',  ( 0.000000000000000000, 0.000000000000000000, 0.000000000000000000 ) ) ;
#8519 = ADVANCED_FACE ( 'NONE', ( #9706 ), #6479, .T. ) ;
#8520 = ORIENTED_EDGE ( 'NONE', *, *, #8193, .T. ) ;
#8521 = CARTESIAN_POINT ( 'NONE',  ( 0.000000000000000000, 9.000000000000000000, 0.000000000000000000 ) ) ;
#8522 = B_SPLINE_CURVE_WITH_KNOTS ( 'NONE', 3,
 ( #8414, #3051, #5197, #3114 ),
 .UNSPECIFIED., .F., .F.,
 ( 4, 4 ),
 ( 0.1547128134717859205, 1.000000000000000000 ),
 .UNSPECIFIED. ) ;
#8523 = DIRECTION ( 'NONE',  ( 1.000000000000000000, 0.000000000000000000, 0.000000000000000000 ) ) ;
#8524 = CARTESIAN_POINT ( 'NONE',  ( 10.86210944460165528, 3.000000000000000000, 29.48017534571043541 ) ) ;
#8525 = CARTESIAN_POINT ( 'NONE',  ( -2.264806262022998062, 3.000000000000000000, -14.82803603298499340 ) ) ;
#8526 = PRODUCT_DEFINITION_SHAPE ( 'NONE', 'NONE',  #13599 ) ;
#8527 = DIRECTION ( 'NONE',  ( 0.000000000000000000, 0.000000000000000000, -1.000000000000000000 ) ) ;
#8528 = DIRECTION ( 'NONE',  ( -0.000000000000000000, -1.000000000000000000, -0.000000000000000000 ) ) ;
#8529 = CARTESIAN_POINT ( 'NONE',  ( -8.883544964652065445, 3.000000000000000000, -12.08646469655229438 ) ) ;
#8530 = ORIENTED_EDGE ( 'NONE', *, *, #11417, .T. ) ;
#8531 = DIRECTION ( 'NONE',  ( 0.000000000000000000, 0.000000000000000000, 1.000000000000000000 ) ) ;
#8532 = EDGE_LOOP ( 'NONE', ( #6305, #2368 ) ) ;
#8533 = ORIENTED_EDGE ( 'NONE', *, *, #11230, .T. ) ;
#8534 = ORIENTED_EDGE ( 'NONE', *, *, #11123, .F. ) ;
#8535 = CARTESIAN_POINT ( 'NONE',  ( -0.5400000000007666445, 3.000000000000000000, -12.07793442604883793 ) ) ;
#8536 = ADVANCED_FACE ( 'NONE', ( #12891 ), #4545, .T. ) ;
#8537 = EDGE_CURVE ( 'NONE', #1515, #8365, #9507, .T. ) ;
#8538 = ORIENTED_EDGE ( 'NONE', *, *, #5163, .F. ) ;
#8539 = SHAPE_REPRESENTATION ( 'gripper', ( #10007 ), #12883 ) ;
#8540 = CARTESIAN_POINT ( 'NONE',  ( -9.379342464487789854, 3.000000000000000000, -10.98198414889931307 ) ) ;
#8541 = DIRECTION ( 'NONE',  ( 0.000000000000000000, 0.000000000000000000, -1.000000000000000000 ) ) ;
#8542 = DIRECTION ( 'NONE',  ( 0.000000000000000000, 0.000000000000000000, 1.000000000000000000 ) ) ;
#8543 = CARTESIAN_POINT ( 'NONE',  ( 0.000000000000000000, 3.000000000000000000, -5.000000000000000000 ) ) ;
#8544 = CARTESIAN_POINT ( 'NONE',  ( -13.27898586450070084, 0.000000000000000000, -5.170206418547585336 ) ) ;
#8545 = FACE_BOUND ( 'NONE', #10357, .T. ) ;
#8546 = DIRECTION ( 'NONE',  ( -0.000000000000000000, -1.000000000000000000, -0.000000000000000000 ) ) ;
#8547 = CARTESIAN_POINT ( 'NONE',  ( -13.27898586450066709, 3.000000000000000000, 5.170206418547661720 ) ) ;
#8548 = ORIENTED_EDGE ( 'NONE', *, *, #11329, .T. ) ;
#8549 = CARTESIAN_POINT ( 'NONE',  ( 0.000000000000000000, 2.900000000000000355, -3.500000000000000888 ) ) ;
#8550 = ORIENTED_EDGE ( 'NONE', *, *, #11417, .F. ) ;
#8551 = VERTEX_POINT ( 'NONE', #8470 ) ;
#8552 = B_SPLINE_CURVE_WITH_KNOTS ( 'NONE', 3,
 ( #7168, #5089, #7229, #10529 ),
 .UNSPECIFIED., .F., .F.,
 ( 4, 4 ),
 ( 0.1547128134717859205, 1.000000000000000000 ),
 .UNSPECIFIED. ) ;
#8553 = ORIENTED_EDGE ( 'NONE', *, *, #5916, .T. ) ;
#8554 = TOROIDAL_SURFACE ( 'NONE', #9665, 1.600000000000000311, 0.1000000000000000056 ) ;
#8555 = DIRECTION ( 'NONE',  ( -0.000000000000000000, -1.000000000000000000, -0.000000000000000000 ) ) ;
#8556 = CARTESIAN_POINT ( 'NONE',  ( -1.105736515254454044, 0.000000000000000000, 13.50994833511691340 ) ) ;
#8557 = CARTESIAN_POINT ( 'NONE',  ( 5.958322434183388694, 9.000000000000000000, -6.062045345451230638 ) ) ;
#8558 = B_SPLINE_CURVE_WITH_KNOTS ( 'NONE', 3,
 ( #8510, #6457, #6523, #3218 ),
 .UNSPECIFIED., .F., .F.,
 ( 4, 4 ),
 ( 0.000000000000000000, 0.5855695330273008592 ),
 .UNSPECIFIED. ) ;
#8559 = CARTESIAN_POINT ( 'NONE',  ( 1.105736515254441388, 3.000000000000000000, -13.50994833511691695 ) ) ;
#8560 = DIRECTION ( 'NONE',  ( 0.000000000000000000, 0.000000000000000000, 1.000000000000000000 ) ) ;
#8561 = CARTESIAN_POINT ( 'NONE',  ( 7.702138240596505092, 3.000000000000000000, -30.99999999999999289 ) ) ;
#8562 = CIRCLE ( 'NONE', #9264, 14.25000000000000000 ) ;
#8563 = ORIENTED_EDGE ( 'NONE', *, *, #6212, .F. ) ;
#8564 = EDGE_CURVE ( 'NONE', #2964, #2682, #2815, .T. ) ;
#8565 = ORIENTED_EDGE ( 'NONE', *, *, #12589, .T. ) ;
#8566 = CARTESIAN_POINT ( 'NONE',  ( 3.469446951953614189E-15, 0.000000000000000000, -7.049999999999999822 ) ) ;
#8567 = MANIFOLD_SOLID_BREP ( 'Base-Flange1', #13019 ) ;
#8568 = VERTEX_POINT ( 'NONE', #8872 ) ;
#8569 = CARTESIAN_POINT ( 'NONE',  ( -9.593885948927676210, 0.000000000000000000, 8.504652361247165615 ) ) ;
#8570 = CIRCLE ( 'NONE', #12563, 12.08999999999737263 ) ;
#8571 = CARTESIAN_POINT ( 'NONE',  ( 10.72979803820131472, 3.000000000000000000, 5.571313494980131509 ) ) ;
#8572 = CARTESIAN_POINT ( 'NONE',  ( 5.571433138827823761, 3.000000000000000000, 10.72973591378220704 ) ) ;
#8573 = CARTESIAN_POINT ( 'NONE',  ( -12.76342233970728124, 0.000000000000000000, -4.564691384634500970 ) ) ;
#8574 = DIRECTION ( 'NONE',  ( 0.000000000000000000, 0.000000000000000000, 1.000000000000000000 ) ) ;
#8575 = ADVANCED_FACE ( 'NONE', ( #5703 ), #5643, .F. ) ;
#8576 = CARTESIAN_POINT ( 'NONE',  ( 0.000000000000000000, 2.900000000000000355, 0.000000000000000000 ) ) ;
#8577 = ADVANCED_FACE ( 'NONE', ( #3642 ), #12276, .T. ) ;
#8578 = DIRECTION ( 'NONE',  ( 0.000000000000000000, 0.000000000000000000, 1.000000000000000000 ) ) ;
#8579 = AXIS2_PLACEMENT_3D ( 'NONE', #13563, #2058, #6252 ) ;
#8580 = VERTEX_POINT ( 'NONE', #558 ) ;
#8581 = ORIENTED_EDGE ( 'NONE', *, *, #11194, .F. ) ;
#8582 = ADVANCED_FACE ( 'NONE', ( #7841 ), #9839, .T. ) ;
#8583 = ORIENTED_EDGE ( 'NONE', *, *, #6244, .T. ) ;
#8584 = CARTESIAN_POINT ( 'NONE',  ( 6.123233995736766282E-16, 0.000000000000000000, -5.000000000000000000 ) ) ;
#8585 = EDGE_CURVE ( 'NONE', #3916, #6405, #623, .T. ) ;
#8586 = ORIENTED_EDGE ( 'NONE', *, *, #427, .T. ) ;
#8587 = FACE_OUTER_BOUND ( 'NONE', #1949, .T. ) ;
#8588 = AXIS2_PLACEMENT_3D ( 'NONE', #2513, #3738, #12092 ) ;
#8589 = CYLINDRICAL_SURFACE ( 'NONE', #11891, 1.500000000000000222 ) ;
#8590 = CIRCLE ( 'NONE', #662, 1.500000000000000666 ) ;
#8591 = DIRECTION ( 'NONE',  ( 0.000000000000000000, 1.000000000000000000, 0.000000000000000000 ) ) ;
#8592 = CARTESIAN_POINT ( 'NONE',  ( -1.958311002203252160, 0.000000000000000000, -14.87484884897975768 ) ) ;
#8593 = ADVANCED_FACE ( 'NONE', ( #3572 ), #4815, .F. ) ;
#8594 = CARTESIAN_POINT ( 'NONE',  ( 1.959434878635765477E-16, 3.000000000000000000, -1.600000000000000311 ) ) ;
#8595 = CARTESIAN_POINT ( 'NONE',  ( 5.452638258930520010, 3.000000000000000000, -13.97385902380752754 ) ) ;
#8596 = ORIENTED_EDGE ( 'NONE', *, *, #10020, .T. ) ;
#8597 = ORIENTED_EDGE ( 'NONE', *, *, #4776, .F. ) ;
#8598 = ORIENTED_EDGE ( 'NONE', *, *, #3563, .T. ) ;
#8599 = EDGE_LOOP ( 'NONE', ( #11904, #11540, #12263, #4375 ) ) ;
#8600 = CARTESIAN_POINT ( 'NONE',  ( 0.000000000000000000, 9.000000000000000000, 0.000000000000000000 ) ) ;
#8601 = ADVANCED_FACE ( 'NONE', ( #10112 ), #2367, .F. ) ;
#8602 = ORIENTED_EDGE ( 'NONE', *, *, #2060, .T. ) ;
#8603 = CARTESIAN_POINT ( 'NONE',  ( 26.30958424017656938, 2.900000000000000355, -4.500000000000000888 ) ) ;
#8604 = CARTESIAN_POINT ( 'NONE',  ( 9.065480927540312095, 3.000000000000000000, -9.324856600128422102 ) ) ;
#8605 = CARTESIAN_POINT ( 'NONE',  ( 31.00000000000000000, 0.09999999999999982514, 0.000000000000000000 ) ) ;
#8606 = DIRECTION ( 'NONE',  ( 0.000000000000000000, 0.000000000000000000, -1.000000000000000000 ) ) ;
#8607 = CARTESIAN_POINT ( 'NONE',  ( 0.000000000000000000, 1.000000000000000000, 0.000000000000000000 ) ) ;
#8608 = VECTOR ( 'NONE', #3013, 1000.000000000000000 ) ;
#8609 = CARTESIAN_POINT ( 'NONE',  ( 2.928250210355320959, 0.000000000000000000, -13.52637830886121506 ) ) ;
#8610 = VECTOR ( 'NONE', #5700, 1000.000000000000000 ) ;
#8611 = EDGE_CURVE ( 'NONE', #3201, #4927, #8796, .T. ) ;
#8612 = CARTESIAN_POINT ( 'NONE',  ( 10.14701493152832512, 3.000000000000000000, -29.73855628788322747 ) ) ;
#8613 = EDGE_CURVE ( 'NONE', #1800, #7580, #9080, .T. ) ;
#8614 = CARTESIAN_POINT ( 'NONE',  ( 8.158651161643900807, 3.000000000000000000, 8.922136023539609440 ) ) ;
#8615 = ORIENTED_EDGE ( 'NONE', *, *, #1274, .T. ) ;
#8616 = DIRECTION ( 'NONE',  ( -0.000000000000000000, -1.000000000000000000, -0.000000000000000000 ) ) ;
#8617 = B_SPLINE_SURFACE_WITH_KNOTS ( 'NONE', 3, 1, ( 
 ( #654, #8974 ),
 ( #2850, #4849 ),
 ( #11261, #9125 ),
 ( #9939, #9044 ) ),
 .UNSPECIFIED., .F., .F., .F.,
 ( 4, 4 ),
 ( 2, 2 ),
 ( 0.1547128134717859205, 1.000000000000000000 ),
 ( 0.000000000000000000, 1.000000000000000000 ),
 .UNSPECIFIED. ) ;
#8618 = EDGE_LOOP ( 'NONE', ( #12607, #3042, #6642, #12825 ) ) ;
#8619 = B_SPLINE_CURVE_WITH_KNOTS ( 'NONE', 3,
 ( #9851, #5714, #7790, #9991 ),
 .UNSPECIFIED., .F., .F.,
 ( 4, 4 ),
 ( 0.000000000000000000, 0.5855695330273008592 ),
 .UNSPECIFIED. ) ;
#8620 = ORIENTED_EDGE ( 'NONE', *, *, #9452, .T. ) ;
#8621 = EDGE_LOOP ( 'NONE', ( #2738, #7645 ) ) ;
#8622 = VECTOR ( 'NONE', #6416, 1000.000000000000114 ) ;
#8623 = AXIS2_PLACEMENT_3D ( 'NONE', #12381, #4787, #5886 ) ;
#8624 = CARTESIAN_POINT ( 'NONE',  ( 5.250000000000000000, 0.000000000000000000, -27.94078293894052578 ) ) ;
#8625 = FACE_OUTER_BOUND ( 'NONE', #3570, .T. ) ;
#8626 = CARTESIAN_POINT ( 'NONE',  ( 0.000000000000000000, 0.000000000000000000, 0.000000000000000000 ) ) ;
#8627 = FACE_OUTER_BOUND ( 'NONE', #6965, .T. ) ;
#8628 = DIRECTION ( 'NONE',  ( 0.000000000000000000, 0.000000000000000000, 1.000000000000000000 ) ) ;
#8629 = EDGE_CURVE ( 'NONE', #11917, #11340, #8306, .T. ) ;
#8630 = CIRCLE ( 'NONE', #13271, 2.999999999999992450 ) ;
#8631 = DIRECTION ( 'NONE',  ( 0.000000000000000000, 1.000000000000000000, -0.000000000000000000 ) ) ;
#8632 = CIRCLE ( 'NONE', #2702, 0.7499999999999997780 ) ;
#8633 =( GEOMETRIC_REPRESENTATION_CONTEXT ( 3 ) GLOBAL_UNCERTAINTY_ASSIGNED_CONTEXT ( ( #7233 ) ) GLOBAL_UNIT_ASSIGNED_CONTEXT ( ( #12750, #6547, #2205 ) ) REPRESENTATION_CONTEXT ( 'NONE', 'WORKASPACE' ) );
#8634 = ORIENTED_EDGE ( 'NONE', *, *, #61, .F. ) ;
#8635 = EDGE_LOOP ( 'NONE', ( #1065, #8837, #6051, #5180 ) ) ;
#8636 = CARTESIAN_POINT ( 'NONE',  ( 8.922226997226887946, 3.000000000000000000, 8.158551673544288008 ) ) ;
#8637 = EDGE_LOOP ( 'NONE', ( #225, #12502, #2907, #7844 ) ) ;
#8638 = FACE_OUTER_BOUND ( 'NONE', #2833, .T. ) ;
#8639 = AXIS2_PLACEMENT_3D ( 'NONE', #3882, #6029, #4922 ) ;
#8640 = PRODUCT_DEFINITION_SHAPE ( 'NONE', 'NONE',  #13598 ) ;
#8641 = VECTOR ( 'NONE', #10498, 1000.000000000000000 ) ;
#8642 = VECTOR ( 'NONE', #1087, 1000.000000000000000 ) ;
#8643 = EDGE_CURVE ( 'NONE', #11321, #8320, #13246, .T. ) ;
#8644 = CARTESIAN_POINT ( 'NONE',  ( 7.771282357155271825, 0.000000000000000000, -3.443424244174282389 ) ) ;
#8645 = B_SPLINE_CURVE_WITH_KNOTS ( 'NONE', 3,
 ( #13108, #9998, #13318, #9923 ),
 .UNSPECIFIED., .F., .F.,
 ( 4, 4 ),
 ( 0.1547128134717859205, 1.000000000000000000 ),
 .UNSPECIFIED. ) ;
#8646 = CYLINDRICAL_SURFACE ( 'NONE', #1984, 0.4000000000000000222 ) ;
#8647 = CARTESIAN_POINT ( 'NONE',  ( -10.72973591378220348, 3.000000000000000000, 5.571433138827830867 ) ) ;
#8648 = CARTESIAN_POINT ( 'NONE',  ( -10.72979803820123479, 3.000000000000000000, -5.571313494980285164 ) ) ;
#8649 = DIRECTION ( 'NONE',  ( 0.000000000000000000, 0.000000000000000000, 1.000000000000000000 ) ) ;
#8650 = FACE_OUTER_BOUND ( 'NONE', #4887, .T. ) ;
#8651 = AXIS2_PLACEMENT_3D ( 'NONE', #2899, #4071, #12431 ) ;
#8652 = ORIENTED_EDGE ( 'NONE', *, *, #12916, .T. ) ;
#8653 = EDGE_LOOP ( 'NONE', ( #4352, #8293, #7367, #7815 ) ) ;
#8654 = VERTEX_POINT ( 'NONE', #2552 ) ;
#8655 = VERTEX_POINT ( 'NONE', #2960 ) ;
#8656 = CARTESIAN_POINT ( 'NONE',  ( -8.482622935103766082, 3.000000000000000000, 9.600126836553263487 ) ) ;
#8657 = ORIENTED_EDGE ( 'NONE', *, *, #11594, .F. ) ;
#8658 = EDGE_CURVE ( 'NONE', #1248, #7910, #2491, .T. ) ;
#8659 = CARTESIAN_POINT ( 'NONE',  ( 29.39270799701850123, 3.000000000000000000, -0.3930766723116408401 ) ) ;
#8661 = ADVANCED_FACE ( 'NONE', ( #8315 ), #4183, .F. ) ;
#8660 = CIRCLE ( 'NONE', #4051, 6.749999999999999112 ) ;
#8662 =( NAMED_UNIT ( * ) PLANE_ANGLE_UNIT ( ) SI_UNIT ( $, .RADIAN. ) );
#8663 = CIRCLE ( 'NONE', #11757, 1.000000000000000888 ) ;
#8664 = CARTESIAN_POINT ( 'NONE',  ( 8.208497377870827449, 3.000000000000000000, -8.550000000000002487 ) ) ;
#8665 = CARTESIAN_POINT ( 'NONE',  ( 45.60964950616533287, 3.000000000000000000, -15.50984893380129392 ) ) ;
#8666 = CARTESIAN_POINT ( 'NONE',  ( 19.65244806805498001, 0.000000000000000000, -5.000000000000000000 ) ) ;
#8667 = CARTESIAN_POINT ( 'NONE',  ( -4.499999999999993783, 3.000000000000000000, 13.39999999999999858 ) ) ;
#8668 = ORIENTED_EDGE ( 'NONE', *, *, #7710, .T. ) ;
#8669 = CARTESIAN_POINT ( 'NONE',  ( 0.000000000000000000, 3.000000000000000000, 0.000000000000000000 ) ) ;
#8670 = ORIENTED_EDGE ( 'NONE', *, *, #678, .T. ) ;
#8671 = ORIENTED_EDGE ( 'NONE', *, *, #8829, .T. ) ;
#8672 = CIRCLE ( 'NONE', #2744, 5.486375544325371223 ) ;
#8673 = ORIENTED_EDGE ( 'NONE', *, *, #5815, .T. ) ;
#8674 = AXIS2_PLACEMENT_3D ( 'NONE', #7007, #6290, #13277 ) ;
#8675 = DIRECTION ( 'NONE',  ( 0.1453943818575021418, -0.000000000000000000, 0.9893737785712106714 ) ) ;
#8676 = AXIS2_PLACEMENT_3D ( 'NONE', #11251, #3937, #11450 ) ;
#8677 = EDGE_LOOP ( 'NONE', ( #6814, #12768, #5888, #10553 ) ) ;
#8678 = ADVANCED_FACE ( 'NONE', ( #9423, #11368 ), #9156, .T. ) ;
#8679 = ORIENTED_EDGE ( 'NONE', *, *, #92, .F. ) ;
#8680 = CARTESIAN_POINT ( 'NONE',  ( 9.375397774054407662, 3.000000000000000000, -11.70905276178460497 ) ) ;
#8681 = DIRECTION ( 'NONE',  ( 0.000000000000000000, 1.000000000000000000, -0.000000000000000000 ) ) ;
#8682 = CARTESIAN_POINT ( 'NONE',  ( -10.97318381393799136, 3.000000000000000000, -6.970598036433411693 ) ) ;
#8683 = B_SPLINE_CURVE_WITH_KNOTS ( 'NONE', 3,
 ( #10426, #13593, #13333, #4148 ),
 .UNSPECIFIED., .F., .F.,
 ( 4, 4 ),
 ( 0.1547128134717859205, 1.000000000000000000 ),
 .UNSPECIFIED. ) ;
#8684 = EDGE_CURVE ( 'NONE', #10793, #7310, #1028, .T. ) ;
#8685 = CARTESIAN_POINT ( 'NONE',  ( -14.82803603298502360, 3.000000000000000000, -2.264806262022826644 ) ) ;
#8686 = AXIS2_PLACEMENT_3D ( 'NONE', #12674, #12732, #7689 ) ;
#8687 = EDGE_CURVE ( 'NONE', #1063, #500, #7653, .T. ) ;
#8688 = DIRECTION ( 'NONE',  ( -0.5795187626277481518, -0.000000000000000000, -0.8149588969772669778 ) ) ;
#8689 = FACE_OUTER_BOUND ( 'NONE', #12129, .T. ) ;
#8690 = ORIENTED_EDGE ( 'NONE', *, *, #4470, .F. ) ;
#8691 = CARTESIAN_POINT ( 'NONE',  ( 5.806472362263156661, 9.000000000000000000, -5.419014975255640465 ) ) ;
#8692 = VERTEX_POINT ( 'NONE', #4057 ) ;
#8693 = ORIENTED_EDGE ( 'NONE', *, *, #3893, .T. ) ;
#8694 = ORIENTED_EDGE ( 'NONE', *, *, #7843, .T. ) ;
#8695 = MECHANICAL_DESIGN_GEOMETRIC_PRESENTATION_REPRESENTATION (  '', ( #12243 ), #1225 ) ;
#8696 = EDGE_CURVE ( 'NONE', #11680, #781, #2504, .T. ) ;
#8697 = DIRECTION ( 'NONE',  ( 0.000000000000000000, 1.000000000000000000, 0.000000000000000000 ) ) ;
#8698 = CARTESIAN_POINT ( 'NONE',  ( 10.25006213149504752, 0.000000000000000000, -9.299128225235653744 ) ) ;
#8699 = APPLICATION_PROTOCOL_DEFINITION ( 'draft international standard', 'automotive_design', 1998, #2741 ) ;
#8700 = CARTESIAN_POINT ( 'NONE',  ( 48.06174015963858892, 3.000000000000000000, -3.086958956539055166 ) ) ;
#8701 = CARTESIAN_POINT ( 'NONE',  ( 5.741477348071313713, 0.000000000000000000, -13.86115248177180703 ) ) ;
#8702 = FACE_OUTER_BOUND ( 'NONE', #10219, .T. ) ;
#8703 = DIRECTION ( 'NONE',  ( -0.000000000000000000, -1.000000000000000000, -0.000000000000000000 ) ) ;
#8704 = CARTESIAN_POINT ( 'NONE',  ( 2.928250210355320959, 3.000000000000000000, -13.52637830886121506 ) ) ;
#8705 = ORIENTED_EDGE ( 'NONE', *, *, #7346, .T. ) ;
#8706 = ORIENTED_EDGE ( 'NONE', *, *, #9107, .F. ) ;
#8707 = DIRECTION ( 'NONE',  ( 0.000000000000000000, 0.000000000000000000, 1.000000000000000000 ) ) ;
#8708 = EDGE_CURVE ( 'NONE', #11432, #97, #8963, .T. ) ;
#8709 = ADVANCED_FACE ( 'NONE', ( #6064 ), #5771, .T. ) ;
#8710 = VERTEX_POINT ( 'NONE', #4959 ) ;
#8711 = CARTESIAN_POINT ( 'NONE',  ( -12.68816982652970893, 3.000000000000000000, 2.830255545554337004 ) ) ;
#8712 = CARTESIAN_POINT ( 'NONE',  ( 7.077546079049268357, 0.000000000000000000, 10.67828022838850544 ) ) ;
#8713 = CARTESIAN_POINT ( 'NONE',  ( -12.75843939030334795, 0.000000000000000000, 4.577511697546079006 ) ) ;
#8714 = CARTESIAN_POINT ( 'NONE',  ( -0.1834773636644435324, 3.000000000000000000, -13.00394737445024873 ) ) ;
#8715 = CARTESIAN_POINT ( 'NONE',  ( 30.73000000000000043, 3.000000000000000000, -3.999999999999999112 ) ) ;
#8716 = DIRECTION ( 'NONE',  ( -1.000000000000000000, 0.000000000000000000, 0.000000000000000000 ) ) ;
#8717 = CARTESIAN_POINT ( 'NONE',  ( 0.000000000000000000, 0.000000000000000000, 0.000000000000000000 ) ) ;
#8718 = FACE_OUTER_BOUND ( 'NONE', #9141, .T. ) ;
#8719 = ORIENTED_EDGE ( 'NONE', *, *, #2320, .T. ) ;
#8720 = ORIENTED_EDGE ( 'NONE', *, *, #2320, .F. ) ;
#8721 = ORIENTED_EDGE ( 'NONE', *, *, #6435, .T. ) ;
#8722 = EDGE_LOOP ( 'NONE', ( #5164, #4157, #1585, #4906 ) ) ;
#8723 = DIRECTION ( 'NONE',  ( -0.000000000000000000, -1.000000000000000000, -0.000000000000000000 ) ) ;
#8724 = B_SPLINE_CURVE_WITH_KNOTS ( 'NONE', 3,
 ( #6956, #13013, #6741, #5638 ),
 .UNSPECIFIED., .F., .F.,
 ( 4, 4 ),
 ( 0.1547128134717859205, 1.000000000000000000 ),
 .UNSPECIFIED. ) ;
#8725 = ORIENTED_EDGE ( 'NONE', *, *, #3694, .F. ) ;
#8726 = CARTESIAN_POINT ( 'NONE',  ( 7.500000000000003553, 3.000000000000000000, 1.399999999999998579 ) ) ;
#8727 = PRESENTATION_STYLE_ASSIGNMENT (( #7573 ) ) ;
#8728 = B_SPLINE_SURFACE_WITH_KNOTS ( 'NONE', 3, 1, ( 
 ( #2589, #12615 ),
 ( #12687, #3164 ),
 ( #7378, #8713 ),
 ( #3229, #11582 ) ),
 .UNSPECIFIED., .F., .F., .F.,
 ( 4, 4 ),
 ( 2, 2 ),
 ( 0.1547128134717859205, 1.000000000000000000 ),
 ( 0.000000000000000000, 1.000000000000000000 ),
 .UNSPECIFIED. ) ;
#8729 = CARTESIAN_POINT ( 'NONE',  ( 8.093005444143644311, 9.000000000000000000, -2.598704077239528676 ) ) ;
#8730 = DIRECTION ( 'NONE',  ( 0.000000000000000000, 0.000000000000000000, 1.000000000000000000 ) ) ;
#8731 = B_SPLINE_CURVE_WITH_KNOTS ( 'NONE', 3,
 ( #5622, #393, #1492, #9199 ),
 .UNSPECIFIED., .F., .F.,
 ( 4, 4 ),
 ( 0.1547128134717859205, 1.000000000000000000 ),
 .UNSPECIFIED. ) ;
#8732 = DIRECTION ( 'NONE',  ( 0.000000000000000000, 0.000000000000000000, -1.000000000000000000 ) ) ;
#8733 = CARTESIAN_POINT ( 'NONE',  ( 31.00000000000000000, 0.09999999999999982514, 1.500000000000003997 ) ) ;
#8734 = VERTEX_POINT ( 'NONE', #11427 ) ;
#8735 = CARTESIAN_POINT ( 'NONE',  ( -10.72973591378220348, 3.000000000000000000, 5.571433138827830867 ) ) ;
#8736 = VERTEX_POINT ( 'NONE', #1994 ) ;
#8737 = UNCERTAINTY_MEASURE_WITH_UNIT (LENGTH_MEASURE( 1.000000000000000082E-05 ), #9898, 'distance_accuracy_value', 'NONE');
#8738 = ADVANCED_FACE ( 'NONE', ( #13369 ), #3676, .F. ) ;
#8739 = ORIENTED_EDGE ( 'NONE', *, *, #6648, .F. ) ;
#8740 = CARTESIAN_POINT ( 'NONE',  ( -12.98835496148321944, 0.000000000000000000, -0.5501230721522551992 ) ) ;
#8741 = ORIENTED_EDGE ( 'NONE', *, *, #6838, .T. ) ;
#8742 = ORIENTED_EDGE ( 'NONE', *, *, #6400, .T. ) ;
#8743 = DIRECTION ( 'NONE',  ( 0.000000000000000000, 1.000000000000000000, 0.000000000000000000 ) ) ;
#8744 = CARTESIAN_POINT ( 'NONE',  ( 2.161962830978677363, 3.000000000000000000, 14.08504230442587613 ) ) ;
#8745 = CARTESIAN_POINT ( 'NONE',  ( 8.883544964651964193, 0.000000000000000000, -12.08646469655236544 ) ) ;
#8746 = LINE ( 'NONE', #4494, #8222 ) ;
#8747 = CARTESIAN_POINT ( 'NONE',  ( -0.8148820470561124463, 0.000000000000000000, 6.700631854488474204 ) ) ;
#8748 = CARTESIAN_POINT ( 'NONE',  ( -7.500000000000000000, 0.000000000000000000, 1.500000000000000666 ) ) ;
#8749 = ORIENTED_EDGE ( 'NONE', *, *, #8021, .F. ) ;
#8750 = DIRECTION ( 'NONE',  ( 0.000000000000000000, 0.000000000000000000, 1.000000000000000000 ) ) ;
#8751 = VERTEX_POINT ( 'NONE', #8119 ) ;
#8752 = ADVANCED_FACE ( 'NONE', ( #12341 ), #7297, .T. ) ;
#8753 = ORIENTED_EDGE ( 'NONE', *, *, #4253, .T. ) ;
#8754 = VERTEX_POINT ( 'NONE', #12417 ) ;
#8755 = EDGE_CURVE ( 'NONE', #6405, #13024, #2236, .T. ) ;
#8756 = EDGE_CURVE ( 'NONE', #9161, #6340, #2717, .T. ) ;
#8757 = LINE ( 'NONE', #12152, #11911 ) ;
#8758 = DIRECTION ( 'NONE',  ( 0.000000000000000000, 1.000000000000000000, 0.000000000000000000 ) ) ;
#8759 = CARTESIAN_POINT ( 'NONE',  ( 11.48836750521728511, 3.000000000000000000, 8.430890348300561499 ) ) ;
#8760 = DIRECTION ( 'NONE',  ( 0.000000000000000000, 0.000000000000000000, 1.000000000000000000 ) ) ;
#8761 = CARTESIAN_POINT ( 'NONE',  ( -11.90284147956865723, 3.000000000000000000, -9.133371500908332052 ) ) ;
#8762 = DIRECTION ( 'NONE',  ( 0.000000000000000000, 0.000000000000000000, 1.000000000000000000 ) ) ;
#8763 = AXIS2_PLACEMENT_3D ( 'NONE', #2826, #9090, #13309 ) ;
#8764 = EDGE_CURVE ( 'NONE', #13244, #12420, #4704, .T. ) ;
#8765 = ORIENTED_EDGE ( 'NONE', *, *, #2532, .F. ) ;
#8766 = VERTEX_POINT ( 'NONE', #9568 ) ;
#8767 = ADVANCED_FACE ( 'NONE', ( #9687 ), #3566, .F. ) ;
#8768 = CARTESIAN_POINT ( 'NONE',  ( -5.452638258930639914, 3.000000000000000000, -13.97385902380748313 ) ) ;
#8769 = EDGE_CURVE ( 'NONE', #11851, #2083, #2126, .T. ) ;
#8770 = VERTEX_POINT ( 'NONE', #10790 ) ;
#8771 = CARTESIAN_POINT ( 'NONE',  ( -6.506620931068619385, 3.000000000000000000, -10.18979803820057306 ) ) ;
#8772 = FACE_OUTER_BOUND ( 'NONE', #9648, .T. ) ;
#8773 = CARTESIAN_POINT ( 'NONE',  ( 30.73000000000000043, 3.000000000000000000, -3.999999999999999112 ) ) ;
#8774 = CARTESIAN_POINT ( 'NONE',  ( 13.50000000000000355, 0.000000000000000000, -8.550000000000000711 ) ) ;
#8775 = DIRECTION ( 'NONE',  ( 0.000000000000000000, 0.000000000000000000, 1.000000000000000000 ) ) ;
#8776 = CARTESIAN_POINT ( 'NONE',  ( -10.97318381393799136, 3.000000000000000000, -6.970598036433411693 ) ) ;
#8777 = DIRECTION ( 'NONE',  ( 0.000000000000000000, 1.000000000000000000, 0.000000000000000000 ) ) ;
#8778 = ADVANCED_FACE ( 'NONE', ( #5422 ), #7640, .F. ) ;
#8779 = DIRECTION ( 'NONE',  ( -0.000000000000000000, -1.000000000000000000, -0.000000000000000000 ) ) ;
#8780 = ORIENTED_EDGE ( 'NONE', *, *, #13446, .F. ) ;
#8781 = ORIENTED_EDGE ( 'NONE', *, *, #4492, .F. ) ;
#8782 = ORIENTED_EDGE ( 'NONE', *, *, #5476, .F. ) ;
#8783 = VERTEX_POINT ( 'NONE', #7429 ) ;
#8784 = CARTESIAN_POINT ( 'NONE',  ( -2.568302020731516588, 3.000000000000000000, -12.56087513340552242 ) ) ;
#8785 = VECTOR ( 'NONE', #1479, 1000.000000000000000 ) ;
#8786 = AXIS2_PLACEMENT_3D ( 'NONE', #11624, #7223, #6247 ) ;
#8787 = ORIENTED_EDGE ( 'NONE', *, *, #2825, .F. ) ;
#8788 = DIRECTION ( 'NONE',  ( -0.000000000000000000, -1.000000000000000000, -0.000000000000000000 ) ) ;
#8789 = LINE ( 'NONE', #10388, #453 ) ;
#8790 = CARTESIAN_POINT ( 'NONE',  ( 7.771282357155271825, 0.000000000000000000, -3.443424244174282389 ) ) ;
#8791 = AXIS2_PLACEMENT_3D ( 'NONE', #534, #12256, #664 ) ;
#8792 = CARTESIAN_POINT ( 'NONE',  ( 1.580708947611199511, 9.000000000000000000, -8.351727918397596540 ) ) ;
#8793 = CIRCLE ( 'NONE', #2643, 14.25000000000000000 ) ;
#8794 = CARTESIAN_POINT ( 'NONE',  ( -10.25006213149496936, 3.000000000000000000, -9.299128225235415712 ) ) ;
#8795 = ORIENTED_EDGE ( 'NONE', *, *, #3563, .F. ) ;
#8796 = LINE ( 'NONE', #13017, #13492 ) ;
#8797 = ORIENTED_EDGE ( 'NONE', *, *, #8257, .T. ) ;
#8798 = ORIENTED_EDGE ( 'NONE', *, *, #3643, .T. ) ;
#8799 = CARTESIAN_POINT ( 'NONE',  ( -12.98835496148321944, 3.000000000000000000, -0.5501230721522551992 ) ) ;
#8800 = VERTEX_POINT ( 'NONE', #2252 ) ;
#8801 = VECTOR ( 'NONE', #5740, 1000.000000000000000 ) ;
#8802 = VERTEX_POINT ( 'NONE', #6462 ) ;
#8803 = VECTOR ( 'NONE', #7358, 1000.000000000000000 ) ;
#8804 = CARTESIAN_POINT ( 'NONE',  ( -14.39763212228013955, 0.000000000000000000, -1.133238802859595884 ) ) ;
#8805 = CARTESIAN_POINT ( 'NONE',  ( -12.30759122141990325, 0.000000000000000000, -6.329356821613475681 ) ) ;
#8806 = ADVANCED_FACE ( 'NONE', ( #8650 ), #2393, .T. ) ;
#8807 = CARTESIAN_POINT ( 'NONE',  ( -12.56843238770841786, 0.000000000000000000, 3.367671042046304741 ) ) ;
#8808 = CARTESIAN_POINT ( 'NONE',  ( -14.20034848914876235, 3.000000000000000000, -2.631756770590732764 ) ) ;
#8809 = DIRECTION ( 'NONE',  ( -0.000000000000000000, -1.000000000000000000, -0.000000000000000000 ) ) ;
#8810 = ORIENTED_EDGE ( 'NONE', *, *, #1541, .F. ) ;
#8811 = B_SPLINE_CURVE_WITH_KNOTS ( 'NONE', 3,
 ( #5367, #152, #6541, #9575 ),
 .UNSPECIFIED., .F., .F.,
 ( 4, 4 ),
 ( 0.000000000000000000, 0.8452273900860258760 ),
 .UNSPECIFIED. ) ;
#8812 = CARTESIAN_POINT ( 'NONE',  ( 0.000000000000000000, 0.000000000000000000, 0.000000000000000000 ) ) ;
#8813 = VECTOR ( 'NONE', #9381, 1000.000000000000000 ) ;
#8814 = ORIENTED_EDGE ( 'NONE', *, *, #11985, .F. ) ;
#8815 = ORIENTED_EDGE ( 'NONE', *, *, #11663, .T. ) ;
#8816 = ORIENTED_EDGE ( 'NONE', *, *, #9416, .F. ) ;
#8817 = CARTESIAN_POINT ( 'NONE',  ( -14.90895795148411374, 3.000000000000000000, -1.650143266773683726 ) ) ;
#8818 = CARTESIAN_POINT ( 'NONE',  ( -0.5398653231797316820, 3.000000000000000000, 12.07794044664754018 ) ) ;
#8819 = AXIS2_PLACEMENT_3D ( 'NONE', #3819, #6778, #8020 ) ;
#8820 = ADVANCED_FACE ( 'NONE', ( #8718 ), #9488, .F. ) ;
#8821 = CARTESIAN_POINT ( 'NONE',  ( -12.07794044664754018, 0.000000000000000000, -0.5398653231797256868 ) ) ;
#8822 = EDGE_CURVE ( 'NONE', #7606, #1409, #6321, .T. ) ;
#8823 = DIRECTION ( 'NONE',  ( -0.6923076923076927347, 0.000000000000000000, 0.7216024245882196597 ) ) ;
#8824 = ITEM_DEFINED_TRANSFORMATION ( 'NONE', 'NONE', #8917,  #10007 ) ;
#8825 = DIRECTION ( 'NONE',  ( 0.000000000000000000, 1.000000000000000000, 0.000000000000000000 ) ) ;
#8826 = CARTESIAN_POINT ( 'NONE',  ( 9.299128225235451239, 0.000000000000000000, -10.25006213149493561 ) ) ;
#8827 = CARTESIAN_POINT ( 'NONE',  ( 12.01285915242476499, 0.000000000000000000, -4.000000001073668265 ) ) ;
#8828 = CYLINDRICAL_SURFACE ( 'NONE', #6860, 14.25000000000000178 ) ;
#8829 = EDGE_CURVE ( 'NONE', #11807, #544, #4925, .T. ) ;
#8830 = ORIENTED_EDGE ( 'NONE', *, *, #2278, .F. ) ;
#8831 = VECTOR ( 'NONE', #7845, 1000.000000000000000 ) ;
#8832 = ORIENTED_EDGE ( 'NONE', *, *, #13393, .T. ) ;
#8833 = AXIS2_PLACEMENT_3D ( 'NONE', #718, #2842, #1823 ) ;
#8834 = VECTOR ( 'NONE', #13541, 1000.000000000000000 ) ;
#8835 = B_SPLINE_SURFACE_WITH_KNOTS ( 'NONE', 3, 1, ( 
 ( #8759, #7736 ),
 ( #12975, #4369 ),
 ( #9868, #11950 ),
 ( #2510, #7542 ) ),
 .UNSPECIFIED., .F., .F., .F.,
 ( 4, 4 ),
 ( 2, 2 ),
 ( 0.000000000000000000, 0.8452273900860258760 ),
 ( 0.000000000000000000, 1.000000000000000000 ),
 .UNSPECIFIED. ) ;
#8836 = MANIFOLD_SOLID_BREP ( 'Boss-Extrude3', #5537 ) ;
#8837 = ORIENTED_EDGE ( 'NONE', *, *, #10197, .F. ) ;
#8838 = CARTESIAN_POINT ( 'NONE',  ( -10.72979803820123479, 0.000000000000000000, -5.571313494980285164 ) ) ;
#8839 = DIRECTION ( 'NONE',  ( 0.000000000000000000, 0.000000000000000000, 1.000000000000000000 ) ) ;
#8840 = EDGE_CURVE ( 'NONE', #688, #8093, #6033, .T. ) ;
#8841 = CYLINDRICAL_SURFACE ( 'NONE', #504, 8.500000000000000000 ) ;
#8842 = AXIS2_PLACEMENT_3D ( 'NONE', #12586, #12526, #6299 ) ;
#8843 = CIRCLE ( 'NONE', #11064, 0.9999999999999997780 ) ;
#8844 = LINE ( 'NONE', #258, #5727 ) ;
#8845 = CARTESIAN_POINT ( 'NONE',  ( 28.54655175640005282, 2.900000000000000355, -2.353846153846155254 ) ) ;
#8846 = EDGE_CURVE ( 'NONE', #13326, #2083, #1089, .T. ) ;
#8847 = CARTESIAN_POINT ( 'NONE',  ( -11.63517940784383775, 0.000000000000000000, -7.494008246337203083 ) ) ;
#8848 = EDGE_CURVE ( 'NONE', #2099, #10532, #2187, .T. ) ;
#8849 = CARTESIAN_POINT ( 'NONE',  ( 0.000000000000000000, 0.09999999999999982514, -1.500000000000000222 ) ) ;
#8850 = CARTESIAN_POINT ( 'NONE',  ( -12.40340517008309185, 3.000000000000000000, -3.893011711613028947 ) ) ;
#8851 = ORIENTED_EDGE ( 'NONE', *, *, #11579, .T. ) ;
#8852 = ORIENTED_EDGE ( 'NONE', *, *, #6982, .F. ) ;
#8853 = ORIENTED_EDGE ( 'NONE', *, *, #11788, .T. ) ;
#8854 = VECTOR ( 'NONE', #5891, 1000.000000000000000 ) ;
#8855 = ORIENTED_EDGE ( 'NONE', *, *, #10486, .F. ) ;
#8856 = CARTESIAN_POINT ( 'NONE',  ( 2.453448243599948952, 3.000000000000000000, -2.353846153846153921 ) ) ;
#8857 = AXIS2_PLACEMENT_3D ( 'NONE', #4988, #12376, #12303 ) ;
#8858 = MECHANICAL_DESIGN_GEOMETRIC_PRESENTATION_REPRESENTATION (  '', ( #5350 ), #4463 ) ;
#8859 = ORIENTED_EDGE ( 'NONE', *, *, #9113, .F. ) ;
#8860 = EDGE_CURVE ( 'NONE', #3264, #8258, #12846, .T. ) ;
#8861 = DIRECTION ( 'NONE',  ( 0.000000000000000000, 1.000000000000000000, 0.000000000000000000 ) ) ;
#8862 = CARTESIAN_POINT ( 'NONE',  ( 8.093005444143644311, 0.000000000000000000, -2.598704077239528676 ) ) ;
#8863 = PLANE ( 'NONE',  #11448 ) ;
#8864 = AXIS2_PLACEMENT_3D ( 'NONE', #8624, #8697, #3462 ) ;
#8865 = CARTESIAN_POINT ( 'NONE',  ( -7.780961115628980629, 9.000000000000000000, -3.421497350147988392 ) ) ;
#8866 = PRODUCT_DEFINITION_SHAPE ( 'NONE', 'NONE',  #13621 ) ;
#8867 = VECTOR ( 'NONE', #1396, 1000.000000000000000 ) ;
#8868 = B_SPLINE_CURVE_WITH_KNOTS ( 'NONE', 3,
 ( #13295, #11155, #11994, #10110 ),
 .UNSPECIFIED., .F., .F.,
 ( 4, 4 ),
 ( 0.09090310649439187207, 0.1203211835519651524 ),
 .UNSPECIFIED. ) ;
#8869 = CARTESIAN_POINT ( 'NONE',  ( -11.52330688609014686, 0.000000000000000000, -6.017756925049552841 ) ) ;
#8870 = CARTESIAN_POINT ( 'NONE',  ( 0.5398653231797245766, 0.000000000000000000, -12.07794044664754018 ) ) ;
#8871 = VERTEX_POINT ( 'NONE', #6941 ) ;
#8872 = CARTESIAN_POINT ( 'NONE',  ( 30.65246752842885058, 3.000000000000000000, -7.988606140548566437 ) ) ;
#8873 = ORIENTED_EDGE ( 'NONE', *, *, #11140, .F. ) ;
#8874 = VERTEX_POINT ( 'NONE', #8850 ) ;
#8875 = LINE ( 'NONE', #9783, #12608 ) ;
#8876 = VERTEX_POINT ( 'NONE', #11899 ) ;
#8877 = AXIS2_PLACEMENT_3D ( 'NONE', #9201, #2940, #13352 ) ;
#8878 = VECTOR ( 'NONE', #6525, 1000.000000000000000 ) ;
#8879 = EDGE_CURVE ( 'NONE', #12419, #144, #461, .T. ) ;
#8880 = VERTEX_POINT ( 'NONE', #2658 ) ;
#8881 = EDGE_CURVE ( 'NONE', #6616, #11941, #5851, .T. ) ;
#8882 = FACE_OUTER_BOUND ( 'NONE', #7414, .T. ) ;
#8883 =( NAMED_UNIT ( * ) PLANE_ANGLE_UNIT ( ) SI_UNIT ( $, .RADIAN. ) );
#8884 = APPLICATION_CONTEXT ( 'automotive_design' ) ;
#8885 = DIRECTION ( 'NONE',  ( 0.000000000000000000, -0.000000000000000000, 1.000000000000000000 ) ) ;
#8886 = DIRECTION ( 'NONE',  ( -0.000000000000000000, -1.000000000000000000, -0.000000000000000000 ) ) ;
#8887 = CARTESIAN_POINT ( 'NONE',  ( -3.542894779577211661, 3.000000000000000000, -12.51336118825813948 ) ) ;
#8888 = DIRECTION ( 'NONE',  ( 0.000000000000000000, 0.000000000000000000, -1.000000000000000000 ) ) ;
#8889 = CARTESIAN_POINT ( 'NONE',  ( -1.119409668803374558, 3.000000000000000000, -13.50845331674225669 ) ) ;
#8890 = ORIENTED_EDGE ( 'NONE', *, *, #1030, .T. ) ;
#8891 = AXIS2_PLACEMENT_3D ( 'NONE', #1331, #2632, #5805 ) ;
#8892 = DIRECTION ( 'NONE',  ( -0.000000000000000000, -1.000000000000000000, -0.000000000000000000 ) ) ;
#8893 = AXIS2_PLACEMENT_3D ( 'NONE', #2497, #8809, #11736 ) ;
#8894 = ORIENTED_EDGE ( 'NONE', *, *, #1522, .T. ) ;
#8895 = VECTOR ( 'NONE', #10221, 1000.000000000000000 ) ;
#8896 = ORIENTED_EDGE ( 'NONE', *, *, #13504, .T. ) ;
#8897 = EDGE_LOOP ( 'NONE', ( #6644, #8742 ) ) ;
#8898 = B_SPLINE_CURVE_WITH_KNOTS ( 'NONE', 3,
 ( #9454, #5255, #13538, #110 ),
 .UNSPECIFIED., .F., .F.,
 ( 4, 4 ),
 ( 0.1547128134717859205, 1.000000000000000000 ),
 .UNSPECIFIED. ) ;
#8899 = CARTESIAN_POINT ( 'NONE',  ( 41.29994854050690378, 0.000000000000000000, -5.141175130212632283 ) ) ;
#8900 = VECTOR ( 'NONE', #1863, 1000.000000000000000 ) ;
#8901 = CARTESIAN_POINT ( 'NONE',  ( -5.733772933379472470, 0.000000000000000000, 13.04554897075799502 ) ) ;
#8902 = FACE_OUTER_BOUND ( 'NONE', #5165, .T. ) ;
#8903 = DIRECTION ( 'NONE',  ( -0.000000000000000000, -1.000000000000000000, -0.000000000000000000 ) ) ;
#8904 = CARTESIAN_POINT ( 'NONE',  ( 0.000000000000000000, 0.000000000000000000, 0.000000000000000000 ) ) ;
#8905 = LINE ( 'NONE', #6842, #12845 ) ;
#8906 = CARTESIAN_POINT ( 'NONE',  ( -9.065441275458884007, 0.000000000000000000, -9.324917484779556176 ) ) ;
#8907 = DIRECTION ( 'NONE',  ( 0.000000000000000000, 1.000000000000000000, 0.000000000000000000 ) ) ;
#8908 = DIRECTION ( 'NONE',  ( -0.000000000000000000, -1.000000000000000000, -0.000000000000000000 ) ) ;
#8909 = CARTESIAN_POINT ( 'NONE',  ( -3.647599401157625376, 3.000000000000000000, -11.52662650599085836 ) ) ;
#8910 = EDGE_LOOP ( 'NONE', ( #8152, #8292, #6598, #3193 ) ) ;
#8911 = EDGE_LOOP ( 'NONE', ( #11753, #8058, #11900, #11306 ) ) ;
#8912 = EDGE_CURVE ( 'NONE', #8499, #11537, #7886, .T. ) ;
#8913 = ORIENTED_EDGE ( 'NONE', *, *, #5636, .F. ) ;
#8914 = LINE ( 'NONE', #11059, #7124 ) ;
#8915 = CARTESIAN_POINT ( 'NONE',  ( 12.00000000000001243, 5.000000000000000000, 7.000000000000000888 ) ) ;
#8916 = B_SPLINE_SURFACE_WITH_KNOTS ( 'NONE', 3, 1, ( 
 ( #5188, #13527 ),
 ( #9387, #12561 ),
 ( #913, #6345 ),
 ( #4351, #9442 ) ),
 .UNSPECIFIED., .F., .F., .F.,
 ( 4, 4 ),
 ( 2, 2 ),
 ( 0.000000000000000000, 0.5855695330273008592 ),
 ( 0.000000000000000000, 1.000000000000000000 ),
 .UNSPECIFIED. ) ;
#8917 = AXIS2_PLACEMENT_3D ( 'NONE', #6057, #4747, #1783 ) ;
#8918 = CARTESIAN_POINT ( 'NONE',  ( 31.00000000000000000, 3.000000000000000000, 3.499999999999999556 ) ) ;
#8919 = CARTESIAN_POINT ( 'NONE',  ( 0.000000000000000000, 0.000000000000000000, 0.000000000000000000 ) ) ;
#8920 = CARTESIAN_POINT ( 'NONE',  ( 5.806472362263156661, 9.000000000000000000, -5.419014975255640465 ) ) ;
#8921 = CARTESIAN_POINT ( 'NONE',  ( 12.46219022525837694, 0.000000000000000000, -4.344528055836598845 ) ) ;
#8922 = DIRECTION ( 'NONE',  ( 0.000000000000000000, 0.000000000000000000, 1.000000000000000000 ) ) ;
#8923 = CARTESIAN_POINT ( 'NONE',  ( 4.163799117101002038E-16, 0.09999999999999982514, -3.400000000000001243 ) ) ;
#8924 = VERTEX_POINT ( 'NONE', #5687 ) ;
#8925 = ADVANCED_FACE ( 'NONE', ( #7964 ), #5897, .T. ) ;
#8926 = VERTEX_POINT ( 'NONE', #4661 ) ;
#8927 = ORIENTED_EDGE ( 'NONE', *, *, #6042, .T. ) ;
#8928 = CARTESIAN_POINT ( 'NONE',  ( 11.90284147956858085, 3.000000000000000000, -9.133371500908429752 ) ) ;
#8929 = ADVANCED_FACE ( 'NONE', ( #6862 ), #10035, .T. ) ;
#8930 = ORIENTED_EDGE ( 'NONE', *, *, #13057, .F. ) ;
#8931 = EDGE_CURVE ( 'NONE', #8734, #8874, #2898, .T. ) ;
#8932 = EDGE_CURVE ( 'NONE', #2502, #4277, #9968, .T. ) ;
#8933 = DIRECTION ( 'NONE',  ( 0.000000000000000000, 0.000000000000000000, -1.000000000000000000 ) ) ;
#8934 = CARTESIAN_POINT ( 'NONE',  ( 28.67696780347061392, 41.33135765298363395, 66.33042399990210924 ) ) ;
#8935 = CARTESIAN_POINT ( 'NONE',  ( 7.146769547044127258, 0.000000000000000000, -1.771712133291270863 ) ) ;
#8936 = CARTESIAN_POINT ( 'NONE',  ( -1.604252589105048976, 0.000000000000000000, -8.347237484961699039 ) ) ;
#8937 = B_SPLINE_CURVE_WITH_KNOTS ( 'NONE', 2,
 ( #3861, #2562, #10895 ),
 .UNSPECIFIED., .F., .F.,
 ( 3, 3 ),
 ( 0.000000000000000000, 1.000000000000000000 ),
 .UNSPECIFIED. ) ;
#8938 = CARTESIAN_POINT ( 'NONE',  ( 7.110882674384088276, 0.000000000000000000, -3.538387050178523729 ) ) ;
#8939 = DIRECTION ( 'NONE',  ( 0.000000000000000000, 1.000000000000000000, -0.000000000000000000 ) ) ;
#8940 = PLANE ( 'NONE',  #5614 ) ;
#8941 = ORIENTED_EDGE ( 'NONE', *, *, #3282, .T. ) ;
#8942 = DIRECTION ( 'NONE',  ( -0.8698071910200015910, 0.000000000000000000, -0.4933917819034833729 ) ) ;
#8943 = EDGE_CURVE ( 'NONE', #7676, #7333, #5790, .T. ) ;
#8944 = ORIENTED_EDGE ( 'NONE', *, *, #11594, .T. ) ;
#8945 = VERTEX_POINT ( 'NONE', #2594 ) ;
#8946 = CARTESIAN_POINT ( 'NONE',  ( -8.430890348300559722, 0.000000000000000000, 11.48836750521728689 ) ) ;
#8947 = ORIENTED_EDGE ( 'NONE', *, *, #10913, .F. ) ;
#8948 = EDGE_CURVE ( 'NONE', #10892, #10888, #3686, .T. ) ;
#8949 = VERTEX_POINT ( 'NONE', #1644 ) ;
#8950 = DIRECTION ( 'NONE',  ( 0.000000000000000000, 0.000000000000000000, -1.000000000000000000 ) ) ;
#8951 = DIRECTION ( 'NONE',  ( 0.000000000000000000, 1.000000000000000000, -0.000000000000000000 ) ) ;
#8952 = SURFACE_STYLE_USAGE ( .BOTH. , #6695 ) ;
#8953 = DIRECTION ( 'NONE',  ( -0.9248782281665499649, 0.000000000000000000, 0.3802634127332040759 ) ) ;
#8954 = CARTESIAN_POINT ( 'NONE',  ( -5.830003112347290184, 9.000000000000000000, -5.394061460138155795 ) ) ;
#8955 = CARTESIAN_POINT ( 'NONE',  ( 1.836970198721030181E-16, 13.00000000000000178, 1.500000000000000222 ) ) ;
#8956 = ORIENTED_EDGE ( 'NONE', *, *, #4222, .T. ) ;
#8957 = CARTESIAN_POINT ( 'NONE',  ( -8.479748006907131597, 9.000000000000000000, 0.5864074857593127854 ) ) ;
#8958 = PRODUCT ( 'gear-link-1', 'gear-link-1', '', ( #884 ) ) ;
#8959 = EDGE_CURVE ( 'NONE', #2737, #11339, #965, .T. ) ;
#8960 = VERTEX_POINT ( 'NONE', #9140 ) ;
#8961 = ADVANCED_FACE ( 'NONE', ( #7077 ), #5008, .F. ) ;
#8962 = ORIENTED_EDGE ( 'NONE', *, *, #2283, .F. ) ;
#8963 = B_SPLINE_CURVE_WITH_KNOTS ( 'NONE', 3,
 ( #7169, #5224, #3915, #963 ),
 .UNSPECIFIED., .F., .F.,
 ( 4, 4 ),
 ( 0.2280192144657617603, 0.8452273900860258760 ),
 .UNSPECIFIED. ) ;
#8964 = VERTEX_POINT ( 'NONE', #13483 ) ;
#8965 = CARTESIAN_POINT ( 'NONE',  ( 3.469446951953614189E-15, 3.000000000000000000, -7.049999999999999822 ) ) ;
#8966 = LINE ( 'NONE', #11391, #121 ) ;
#8967 = CARTESIAN_POINT ( 'NONE',  ( -8.883544964652065445, 0.000000000000000000, -12.08646469655229438 ) ) ;
#8968 = CARTESIAN_POINT ( 'NONE',  ( -12.25282671965375236, 0.000000000000000000, 5.797378255456025364 ) ) ;
#8969 = LINE ( 'NONE', #438, #9894 ) ;
#8970 = CARTESIAN_POINT ( 'NONE',  ( 3.850308450823737516, 0.000000000000000000, 5.544152309732777617 ) ) ;
#8971 = DIRECTION ( 'NONE',  ( 0.000000000000000000, 0.000000000000000000, -1.000000000000000000 ) ) ;
#8972 = LINE ( 'NONE', #2784, #11472 ) ;
#8973 = DIRECTION ( 'NONE',  ( -0.000000000000000000, -1.000000000000000000, -0.000000000000000000 ) ) ;
#8974 = CARTESIAN_POINT ( 'NONE',  ( -3.647599401157691545, 0.000000000000000000, -11.52662650599084238 ) ) ;
#8975 = ORIENTED_EDGE ( 'NONE', *, *, #10785, .T. ) ;
#8976 = VERTEX_POINT ( 'NONE', #12324 ) ;
#8977 = ORIENTED_EDGE ( 'NONE', *, *, #11223, .T. ) ;
#8978 = CARTESIAN_POINT ( 'NONE',  ( 10.72973591378220704, 0.000000000000000000, -5.571433138827823761 ) ) ;
#8979 = CARTESIAN_POINT ( 'NONE',  ( -6.660869762029062890, 0.000000000000000000, -11.17001010193236610 ) ) ;
#8980 = CARTESIAN_POINT ( 'NONE',  ( -5.571313494980134173, 3.000000000000000000, 10.72979803820131295 ) ) ;
#8981 = DIRECTION ( 'NONE',  ( 0.000000000000000000, 0.000000000000000000, 1.000000000000000000 ) ) ;
#8982 = CARTESIAN_POINT ( 'NONE',  ( -11.80612203322752585, 3.000000000000000000, 2.604531154829235362 ) ) ;
#8983 = EDGE_CURVE ( 'NONE', #10283, #7762, #9202, .T. ) ;
#8984 = CARTESIAN_POINT ( 'NONE',  ( 0.000000000000000000, 3.000000000000000000, 0.000000000000000000 ) ) ;
#8985 = DIRECTION ( 'NONE',  ( -0.000000000000000000, -1.000000000000000000, 0.000000000000000000 ) ) ;
#8986 = CARTESIAN_POINT ( 'NONE',  ( 12.89546620003432764, 0.000000000000000000, -4.733530556166651415 ) ) ;
#8987 = ORIENTED_EDGE ( 'NONE', *, *, #210, .F. ) ;
#8988 = VERTEX_POINT ( 'NONE', #11352 ) ;
#8989 = ORIENTED_EDGE ( 'NONE', *, *, #13420, .T. ) ;
#8990 = CARTESIAN_POINT ( 'NONE',  ( -0.5501230721523990841, 0.000000000000000000, -12.98835496148299384 ) ) ;
#8991 = ORIENTED_EDGE ( 'NONE', *, *, #5242, .F. ) ;
#8992 = CIRCLE ( 'NONE', #9875, 12.00000000000000000 ) ;
#8993 = CARTESIAN_POINT ( 'NONE',  ( 10.33484986938308481, 0.000000000000000000, -8.771102293099065861 ) ) ;
#8994 = DIRECTION ( 'NONE',  ( 0.000000000000000000, 0.000000000000000000, 1.000000000000000000 ) ) ;
#8995 = EDGE_CURVE ( 'NONE', #7605, #11130, #3367, .T. ) ;
#8996 = CARTESIAN_POINT ( 'NONE',  ( 1.836970198721030181E-16, 3.000000000000000000, 1.500000000000000222 ) ) ;
#8997 = LINE ( 'NONE', #1722, #9689 ) ;
#8998 = EDGE_CURVE ( 'NONE', #12420, #911, #3821, .T. ) ;
#8999 = FACE_BOUND ( 'NONE', #119, .T. ) ;
#9000 = CARTESIAN_POINT ( 'NONE',  ( 55.44259468463320673, 3.000000000000000000, -4.702937446762657459 ) ) ;
#9001 = CARTESIAN_POINT ( 'NONE',  ( 7.500000000000003553, 3.000000000000000000, 13.39999999999999858 ) ) ;
#9002 = VERTEX_POINT ( 'NONE', #5144 ) ;
#9003 = DIRECTION ( 'NONE',  ( -0.4933917819034833174, 0.000000000000000000, 0.8698071910200014800 ) ) ;
#9004 = EDGE_CURVE ( 'NONE', #12045, #12265, #2941, .T. ) ;
#9005 = VECTOR ( 'NONE', #4716, 1000.000000000000000 ) ;
#9006 = ORIENTED_EDGE ( 'NONE', *, *, #2867, .F. ) ;
#9007 = AXIS2_PLACEMENT_3D ( 'NONE', #7323, #13461, #4016 ) ;
#9008 = ORIENTED_EDGE ( 'NONE', *, *, #13161, .F. ) ;
#9009 = CARTESIAN_POINT ( 'NONE',  ( 10.00000000000000178, 2.000000000000000000, 10.00000000000000000 ) ) ;
#9010 = VERTEX_POINT ( 'NONE', #11278 ) ;
#9011 = CARTESIAN_POINT ( 'NONE',  ( 0.000000000000000000, 3.000000000000000000, 0.000000000000000000 ) ) ;
#9012 = EDGE_LOOP ( 'NONE', ( #9386, #13344 ) ) ;
#9013 = CARTESIAN_POINT ( 'NONE',  ( -10.69794375946289655, 0.000000000000000000, -7.065816209474156118 ) ) ;
#9014 = CIRCLE ( 'NONE', #4403, 1.000000000000000888 ) ;
#9015 = CYLINDRICAL_SURFACE ( 'NONE', #1379, 0.4000000000000000222 ) ;
#9016 = EDGE_CURVE ( 'NONE', #4277, #1864, #4022, .T. ) ;
#9017 = CARTESIAN_POINT ( 'NONE',  ( 1.119409668803368119, 3.000000000000000000, 13.50845331674225847 ) ) ;
#9018 = VECTOR ( 'NONE', #3862, 1000.000000000000000 ) ;
#9019 = DIRECTION ( 'NONE',  ( -1.000000000000000000, 0.000000000000000000, 0.000000000000000000 ) ) ;
#9020 = ADVANCED_FACE ( 'NONE', ( #8164 ), #2065, .T. ) ;
#9021 = CARTESIAN_POINT ( 'NONE',  ( -0.4399887592034530392, 0.000000000000000000, 8.488604708182295511 ) ) ;
#9022 = CARTESIAN_POINT ( 'NONE',  ( 1.557181465540758758, 0.000000000000000000, 14.16466328168009881 ) ) ;
#9023 = ORIENTED_EDGE ( 'NONE', *, *, #8879, .T. ) ;
#9024 = DIRECTION ( 'NONE',  ( 0.000000000000000000, 1.000000000000000000, -0.000000000000000000 ) ) ;
#9025 = ADVANCED_FACE ( 'NONE', ( #13414 ), #2241, .F. ) ;
#9026 = ORIENTED_EDGE ( 'NONE', *, *, #8171, .F. ) ;
#9027 = ORIENTED_EDGE ( 'NONE', *, *, #11300, .F. ) ;
#9028 = CARTESIAN_POINT ( 'NONE',  ( -2.411622991978541464, 9.000000000000000000, -6.304488444319688689 ) ) ;
#9029 = AXIS2_PLACEMENT_3D ( 'NONE', #5684, #11894, #4590 ) ;
#9030 = AXIS2_PLACEMENT_3D ( 'NONE', #9621, #3346, #2328 ) ;
#9031 = VERTEX_POINT ( 'NONE', #3965 ) ;
#9032 = LINE ( 'NONE', #2506, #764 ) ;
#9033 = CARTESIAN_POINT ( 'NONE',  ( -10.18979803820068675, 3.000000000000000000, 6.506620931068438196 ) ) ;
#9034 = EDGE_CURVE ( 'NONE', #2212, #5259, #6173, .T. ) ;
#9035 = CARTESIAN_POINT ( 'NONE',  ( -12.98835496148321944, 0.000000000000000000, -0.5501230721522551992 ) ) ;
#9036 = EDGE_CURVE ( 'NONE', #5615, #7453, #13286, .T. ) ;
#9037 = LINE ( 'NONE', #5946, #892 ) ;
#9038 = ITEM_DEFINED_TRANSFORMATION ( 'NONE', 'NONE', #4098,  #10007 ) ;
#9039 = CYLINDRICAL_SURFACE ( 'NONE', #3365, 1.500000000000000222 ) ;
#9040 = VECTOR ( 'NONE', #7058, 1000.000000000000000 ) ;
#9041 = DIRECTION ( 'NONE',  ( 0.000000000000000000, 0.000000000000000000, 1.000000000000000000 ) ) ;
#9042 = LINE ( 'NONE', #652, #7942 ) ;
#9043 = DIRECTION ( 'NONE',  ( -0.000000000000000000, -1.000000000000000000, -0.000000000000000000 ) ) ;
#9044 = CARTESIAN_POINT ( 'NONE',  ( -5.170206418547658167, 0.000000000000000000, -13.27898586450066887 ) ) ;
#9045 = B_SPLINE_CURVE_WITH_KNOTS ( 'NONE', 3,
 ( #8314, #4055, #9287, #6062 ),
 .UNSPECIFIED., .F., .F.,
 ( 4, 4 ),
 ( 0.1276832474596248101, 1.000000000000000000 ),
 .UNSPECIFIED. ) ;
#9046 = VERTEX_POINT ( 'NONE', #13354 ) ;
#9047 = ORIENTED_EDGE ( 'NONE', *, *, #11388, .F. ) ;
#9048 = EDGE_LOOP ( 'NONE', ( #8063, #3002, #5688, #4958 ) ) ;
#9049 = CARTESIAN_POINT ( 'NONE',  ( 10.72973591378220704, 3.000000000000000000, -5.571433138827823761 ) ) ;
#9050 = B_SPLINE_CURVE_WITH_KNOTS ( 'NONE', 3,
 ( #12038, #10862, #9820, #1429 ),
 .UNSPECIFIED., .F., .F.,
 ( 4, 4 ),
 ( 0.000000000000000000, 0.8724294488011757887 ),
 .UNSPECIFIED. ) ;
#9051 = FACE_OUTER_BOUND ( 'NONE', #2836, .T. ) ;
#9052 = B_SPLINE_CURVE_WITH_KNOTS ( 'NONE', 3,
 ( #5567, #1101, #3231, #2342 ),
 .UNSPECIFIED., .F., .F.,
 ( 4, 4 ),
 ( 0.1547128134717859205, 1.000000000000000000 ),
 .UNSPECIFIED. ) ;
#9053 = EDGE_CURVE ( 'NONE', #8692, #1419, #12259, .T. ) ;
#9054 = LINE ( 'NONE', #13272, #7547 ) ;
#9055 = CARTESIAN_POINT ( 'NONE',  ( 20.00000000000001776, 6.749999999999972466, -5.112321917994366767E-15 ) ) ;
#9056 = CARTESIAN_POINT ( 'NONE',  ( 6.509732753943064054, 9.000000000000000000, -3.441899519755141412 ) ) ;
#9057 = CARTESIAN_POINT ( 'NONE',  ( 7.771282357155270937, 9.000000000000000000, -3.443424244174282833 ) ) ;
#9058 = AXIS2_PLACEMENT_3D ( 'NONE', #2881, #3208, #11615 ) ;
#9059 = CARTESIAN_POINT ( 'NONE',  ( 3.542895259386137585, 3.000000000000000000, -12.51336047125611017 ) ) ;
#9060 = DIRECTION ( 'NONE',  ( -0.5610724890695777400, 0.000000000000000000, 0.8277666712360849388 ) ) ;
#9061 = EDGE_LOOP ( 'NONE', ( #13384, #1277, #11263, #8987 ) ) ;
#9062 = ORIENTED_EDGE ( 'NONE', *, *, #5005, .F. ) ;
#9063 = ORIENTED_EDGE ( 'NONE', *, *, #10527, .T. ) ;
#9064 = LINE ( 'NONE', #8108, #5338 ) ;
#9065 =( REPRESENTATION_RELATIONSHIP ('NONE','NONE', #3798, #8461 ) REPRESENTATION_RELATIONSHIP_WITH_TRANSFORMATION ( #1827 )SHAPE_REPRESENTATION_RELATIONSHIP( ) );
#9066 = ORIENTED_EDGE ( 'NONE', *, *, #4072, .T. ) ;
#9067 = AXIS2_PLACEMENT_3D ( 'NONE', #7236, #3088, #4062 ) ;
#9068 = CIRCLE ( 'NONE', #10399, 3.500000000000000888 ) ;
#9069 = DIRECTION ( 'NONE',  ( -0.000000000000000000, -1.000000000000000000, -0.000000000000000000 ) ) ;
#9070 = CARTESIAN_POINT ( 'NONE',  ( 28.67696780347059970, 35.33135765298362685, 42.05042399990210811 ) ) ;
#9071 = CARTESIAN_POINT ( 'NONE',  ( 0.000000000000000000, 0.000000000000000000, 0.000000000000000000 ) ) ;
#9072 = FACE_OUTER_BOUND ( 'NONE', #5328, .T. ) ;
#9073 = DIRECTION ( 'NONE',  ( 1.000000000000000000, 0.000000000000000000, 1.224646799147353207E-16 ) ) ;
#9074 = CARTESIAN_POINT ( 'NONE',  ( 48.06174015963858892, 3.000000000000000000, -3.086958956539055166 ) ) ;
#9075 = DIRECTION ( 'NONE',  ( 3.061616997868383141E-16, 0.000000000000000000, 1.000000000000000000 ) ) ;
#9076 = EDGE_LOOP ( 'NONE', ( #11790, #449, #11665, #966 ) ) ;
#9077 = VECTOR ( 'NONE', #6053, 1000.000000000000000 ) ;
#9078 = DIRECTION ( 'NONE',  ( 0.000000000000000000, 0.000000000000000000, 1.000000000000000000 ) ) ;
#9079 = VECTOR ( 'NONE', #13548, 1000.000000000000000 ) ;
#9080 = CIRCLE ( 'NONE', #6671, 12.08999999999737440 ) ;
#9081 = ORIENTED_EDGE ( 'NONE', *, *, #1207, .T. ) ;
#9082 = AXIS2_PLACEMENT_3D ( 'NONE', #1525, #7914, #10957 ) ;
#9083 = ORIENTED_EDGE ( 'NONE', *, *, #9633, .F. ) ;
#9084 = CARTESIAN_POINT ( 'NONE',  ( -14.87484884897978077, 3.000000000000000000, -1.958311002203079187 ) ) ;
#9085 = ADVANCED_FACE ( 'NONE', ( #9270 ), #3337, .F. ) ;
#9086 = ORIENTED_EDGE ( 'NONE', *, *, #2867, .T. ) ;
#9087 = EDGE_CURVE ( 'NONE', #1251, #7638, #4898, .T. ) ;
#9088 = CARTESIAN_POINT ( 'NONE',  ( 3.188443874008702661, 0.000000000000000000, -12.60833581801614578 ) ) ;
#9089 = ORIENTED_EDGE ( 'NONE', *, *, #10984, .T. ) ;
#9090 = DIRECTION ( 'NONE',  ( 0.000000000000000000, 1.000000000000000000, -0.000000000000000000 ) ) ;
#9091 = AXIS2_PLACEMENT_3D ( 'NONE', #10024, #7816, #3678 ) ;
#9092 = VECTOR ( 'NONE', #5450, 1000.000000000000000 ) ;
#9093=STYLED_ITEM('',(#13649),#8836);
#9094 = CARTESIAN_POINT ( 'NONE',  ( -6.934601996837493232, -1.694065894508600678E-18, 3.871968458191308748 ) ) ;
#9095 = B_SPLINE_SURFACE_WITH_KNOTS ( 'NONE', 3, 1, ( 
 ( #11457, #1960 ),
 ( #9453, #4152 ),
 ( #7327, #13397 ),
 ( #6152, #36 ) ),
 .UNSPECIFIED., .F., .F., .F.,
 ( 4, 4 ),
 ( 2, 2 ),
 ( 0.1276832474596244493, 1.000000000000000000 ),
 ( 0.000000000000000000, 1.000000000000000000 ),
 .UNSPECIFIED. ) ;
#9096 = CARTESIAN_POINT ( 'NONE',  ( -2.375523406013125616, 0.000000000000000000, 6.318179211409232998 ) ) ;
#9097 = CARTESIAN_POINT ( 'NONE',  ( -7.155006492985575228, 9.000000000000000000, -1.740452503570284915 ) ) ;
#9098 = CARTESIAN_POINT ( 'NONE',  ( -7.235926821844430812, 0.000000000000000000, 4.459973433655439301 ) ) ;
#9099 = DIRECTION ( 'NONE',  ( 0.000000000000000000, 0.000000000000000000, 1.000000000000000000 ) ) ;
#9100 = ORIENTED_EDGE ( 'NONE', *, *, #12605, .F. ) ;
#9101 = DIRECTION ( 'NONE',  ( 0.000000000000000000, 1.000000000000000000, -0.000000000000000000 ) ) ;
#9102 = EDGE_LOOP ( 'NONE', ( #13139, #11483 ) ) ;
#9103 = VECTOR ( 'NONE', #4737, 1000.000000000000000 ) ;
#9104 = ORIENTED_EDGE ( 'NONE', *, *, #12088, .T. ) ;
#9105 = AXIS2_PLACEMENT_3D ( 'NONE', #10961, #9019, #8070 ) ;
#9106 = CARTESIAN_POINT ( 'NONE',  ( 6.553553527263006551, 1.734723475976807094E-15, 1.616612558808879774 ) ) ;
#9107 = EDGE_CURVE ( 'NONE', #12419, #899, #5173, .T. ) ;
#9108 = EDGE_CURVE ( 'NONE', #933, #4948, #1599, .T. ) ;
#9109 = ORIENTED_EDGE ( 'NONE', *, *, #5186, .F. ) ;
#9110 = FACE_OUTER_BOUND ( 'NONE', #8910, .T. ) ;
#9111 = ADVANCED_FACE ( 'NONE', ( #8902 ), #2575, .F. ) ;
#9112 = CARTESIAN_POINT ( 'NONE',  ( -14.08504230442587790, 3.000000000000000000, -2.161962830978695571 ) ) ;
#9113 = EDGE_CURVE ( 'NONE', #5803, #8184, #12300, .T. ) ;
#9114 = CARTESIAN_POINT ( 'NONE',  ( 0.000000000000000000, 3.000000000000000000, 0.000000000000000000 ) ) ;
#9115 = CARTESIAN_POINT ( 'NONE',  ( -11.46814821560793440, 0.000000000000000000, 5.731782959214994477 ) ) ;
#9116 = CARTESIAN_POINT ( 'NONE',  ( 3.061616997868383141E-16, 13.00000000000000178, 2.500000000000000000 ) ) ;
#9117 = CIRCLE ( 'NONE', #9562, 0.09999999999999982514 ) ;
#9118 = DIRECTION ( 'NONE',  ( -0.000000000000000000, -1.000000000000000000, -0.000000000000000000 ) ) ;
#9119 = VECTOR ( 'NONE', #201, 1000.000000000000000 ) ;
#9120 = DIRECTION ( 'NONE',  ( -2.602085213965207190E-16, 8.673617379884034239E-17, -1.000000000000000000 ) ) ;
#9121 = CARTESIAN_POINT ( 'NONE',  ( 13.50000000000000355, 3.000000000000000000, -7.050000000000000711 ) ) ;
#9122 = VECTOR ( 'NONE', #9847, 1000.000000000000000 ) ;
#9123 = B_SPLINE_CURVE_WITH_KNOTS ( 'NONE', 3,
 ( #7129, #7256, #11327, #4147 ),
 .UNSPECIFIED., .F., .F.,
 ( 4, 4 ),
 ( 0.000000000000000000, 0.8724294488011765658 ),
 .UNSPECIFIED. ) ;
#9124 = FACE_OUTER_BOUND ( 'NONE', #10396, .T. ) ;
#9125 = CARTESIAN_POINT ( 'NONE',  ( -4.577511697546077230, 0.000000000000000000, -12.75843939030334795 ) ) ;
#9126 = ORIENTED_EDGE ( 'NONE', *, *, #3703, .F. ) ;
#9127 = ORIENTED_EDGE ( 'NONE', *, *, #2977, .T. ) ;
#9128 = VERTEX_POINT ( 'NONE', #8821 ) ;
#9129 = AXIS2_PLACEMENT_3D ( 'NONE', #11451, #9391, #2088 ) ;
#9130 = CIRCLE ( 'NONE', #5824, 0.09999999999999982514 ) ;
#9131 = ORIENTED_EDGE ( 'NONE', *, *, #6306, .F. ) ;
#9132 = DIRECTION ( 'NONE',  ( 0.000000000000000000, 0.000000000000000000, -1.000000000000000000 ) ) ;
#9133 =( NAMED_UNIT ( * ) SI_UNIT ( $, .STERADIAN. ) SOLID_ANGLE_UNIT ( ) );
#9134 = LINE ( 'NONE', #739, #6882 ) ;
#9135 = CARTESIAN_POINT ( 'NONE',  ( -11.70905276178463872, 0.000000000000000000, -9.375397774054366806 ) ) ;
#9136 = CARTESIAN_POINT ( 'NONE',  ( -2.928250210355484828, 3.000000000000000000, -13.52637830886140335 ) ) ;
#9137 = AXIS2_PLACEMENT_3D ( 'NONE', #13360, #9971, #8175 ) ;
#9138 = CIRCLE ( 'NONE', #8686, 4.390701948131951582 ) ;
#9139 = CARTESIAN_POINT ( 'NONE',  ( -12.07794044664754018, 3.000000000000000000, -0.5398653231797256868 ) ) ;
#9140 = CARTESIAN_POINT ( 'NONE',  ( 11.70905276178455878, 0.000000000000000000, -9.375397774054460953 ) ) ;
#9141 = EDGE_LOOP ( 'NONE', ( #6672, #1744, #11772, #384 ) ) ;
#9142 = ADVANCED_FACE ( 'NONE', ( #4840 ), #2706, .F. ) ;
#9143 = CYLINDRICAL_SURFACE ( 'NONE', #12807, 12.08999999999737440 ) ;
#9144 = EDGE_CURVE ( 'NONE', #6668, #313, #7864, .T. ) ;
#9145 = DIRECTION ( 'NONE',  ( -0.000000000000000000, -1.000000000000000000, -0.000000000000000000 ) ) ;
#9146 = VECTOR ( 'NONE', #5997, 1000.000000000000000 ) ;
#9147 = ORIENTED_EDGE ( 'NONE', *, *, #8448, .T. ) ;
#9148 = CARTESIAN_POINT ( 'NONE',  ( 0.000000000000000000, 0.000000000000000000, 0.000000000000000000 ) ) ;
#9149 = DIRECTION ( 'NONE',  ( 0.000000000000000000, 0.000000000000000000, 1.000000000000000000 ) ) ;
#9150 = DIRECTION ( 'NONE',  ( -0.000000000000000000, -1.000000000000000000, -0.000000000000000000 ) ) ;
#9151 = CARTESIAN_POINT ( 'NONE',  ( 0.000000000000000000, 0.000000000000000000, -1.500000000000000222 ) ) ;
#9152 = CARTESIAN_POINT ( 'NONE',  ( 0.000000000000000000, 0.09999999999999982514, 0.000000000000000000 ) ) ;
#9153 = CARTESIAN_POINT ( 'NONE',  ( 8.914835885878220623, 0.000000000000000000, -11.11702303352196708 ) ) ;
#9154 = CARTESIAN_POINT ( 'NONE',  ( -6.558450276537426404, 0.000000000000000000, -1.596630818375423866 ) ) ;
#9155 = ORIENTED_EDGE ( 'NONE', *, *, #10713, .T. ) ;
#9156 = PLANE ( 'NONE',  #3585 ) ;
#9157 =( REPRESENTATION_RELATIONSHIP ('NONE','NONE', #3798, #6537 ) REPRESENTATION_RELATIONSHIP_WITH_TRANSFORMATION ( #4712 )SHAPE_REPRESENTATION_RELATIONSHIP( ) );
#9158 = ORIENTED_EDGE ( 'NONE', *, *, #4091, .T. ) ;
#9159 = ORIENTED_EDGE ( 'NONE', *, *, #11832, .F. ) ;
#9160 = CARTESIAN_POINT ( 'NONE',  ( -2.928250210355484828, 3.000000000000000000, -13.52637830886140335 ) ) ;
#9161 = VERTEX_POINT ( 'NONE', #10010 ) ;
#9162 = ORIENTED_EDGE ( 'NONE', *, *, #12173, .T. ) ;
#9163 = LINE ( 'NONE', #1737, #4373 ) ;
#9164 = CARTESIAN_POINT ( 'NONE',  ( -12.68816982652970893, 0.000000000000000000, 2.830255545554337004 ) ) ;
#9165 = DIRECTION ( 'NONE',  ( -0.000000000000000000, -1.000000000000000000, -0.000000000000000000 ) ) ;
#9166 = CARTESIAN_POINT ( 'NONE',  ( 3.000000000000001776, 2.000000000000000000, 7.000000000000000000 ) ) ;
#9167 = CYLINDRICAL_SURFACE ( 'NONE', #11923, 8.499999999999992895 ) ;
#9168 = CARTESIAN_POINT ( 'NONE',  ( 31.00000000000000000, 2.900000000000000355, 1.500000000000003997 ) ) ;
#9169 = EDGE_CURVE ( 'NONE', #5374, #11838, #6871, .T. ) ;
#9170 = EDGE_LOOP ( 'NONE', ( #5035, #9089, #3172, #9374 ) ) ;
#9171 = DIRECTION ( 'NONE',  ( 0.000000000000000000, 0.000000000000000000, 1.000000000000000000 ) ) ;
#9172 = ORIENTED_EDGE ( 'NONE', *, *, #7, .F. ) ;
#9173 = ORIENTED_EDGE ( 'NONE', *, *, #4313, .F. ) ;
#9174 = CARTESIAN_POINT ( 'NONE',  ( -20.74285254778206067, 3.000000000000000000, 14.10762559394868099 ) ) ;
#9175 = ORIENTED_EDGE ( 'NONE', *, *, #3341, .T. ) ;
#9176 = CARTESIAN_POINT ( 'NONE',  ( 50.46378962010818015, 0.000000000000000000, -4.178819016005276943 ) ) ;
#9177 = FACE_OUTER_BOUND ( 'NONE', #12202, .T. ) ;
#9178 = DIRECTION ( 'NONE',  ( 0.000000000000000000, 0.000000000000000000, 1.000000000000000000 ) ) ;
#9179 = CARTESIAN_POINT ( 'NONE',  ( 9.250000000000001776, 1.999999999999998224, 10.00000000000000000 ) ) ;
#9180 = FACE_OUTER_BOUND ( 'NONE', #13002, .T. ) ;
#9181 = CARTESIAN_POINT ( 'NONE',  ( 31.00000000000000000, 2.900000000000000355, 0.000000000000000000 ) ) ;
#9182 = CARTESIAN_POINT ( 'NONE',  ( -13.27898586450066709, 0.000000000000000000, 5.170206418547661720 ) ) ;
#9183 = CARTESIAN_POINT ( 'NONE',  ( -13.73660796332618261, 3.000000000000000000, -6.025412986832017204 ) ) ;
#9184 = EDGE_CURVE ( 'NONE', #7012, #3254, #2467, .T. ) ;
#9185 = CARTESIAN_POINT ( 'NONE',  ( -11.11702303352192445, 3.000000000000000000, 8.914835885878272137 ) ) ;
#9186 = FACE_OUTER_BOUND ( 'NONE', #3376, .T. ) ;
#9187 = ORIENTED_EDGE ( 'NONE', *, *, #7913, .T. ) ;
#9188 = EDGE_CURVE ( 'NONE', #1159, #10417, #5334, .T. ) ;
#9189 = EDGE_LOOP ( 'NONE', ( #12890, #8690, #12942, #768 ) ) ;
#9190 = ADVANCED_FACE ( 'NONE', ( #2633 ), #10942, .F. ) ;
#9191 = ORIENTED_EDGE ( 'NONE', *, *, #2977, .F. ) ;
#9192 = ORIENTED_EDGE ( 'NONE', *, *, #6435, .F. ) ;
#9193 = B_SPLINE_CURVE_WITH_KNOTS ( 'NONE', 3,
 ( #2848, #6027, #4641, #12030 ),
 .UNSPECIFIED., .F., .F.,
 ( 4, 4 ),
 ( 0.000000000000000000, 0.8452273900860258760 ),
 .UNSPECIFIED. ) ;
#9194 = DIRECTION ( 'NONE',  ( 0.000000000000000000, 0.000000000000000000, 1.000000000000000000 ) ) ;
#9195 = DIRECTION ( 'NONE',  ( 0.6923076923076904032, -0.000000000000000000, 0.7216024245882218802 ) ) ;
#9196 = B_SPLINE_CURVE_WITH_KNOTS ( 'NONE', 3,
 ( #1771, #6109, #12396, #10248 ),
 .UNSPECIFIED., .F., .F.,
 ( 4, 4 ),
 ( 0.000000000000000000, 0.5855695330273008592 ),
 .UNSPECIFIED. ) ;
#9197 = LINE ( 'NONE', #8918, #11063 ) ;
#9198 = EDGE_CURVE ( 'NONE', #75, #3196, #6433, .T. ) ;
#9199 = CARTESIAN_POINT ( 'NONE',  ( -14.16466328168009881, 0.000000000000000000, 1.557181465540760534 ) ) ;
#9200 = CARTESIAN_POINT ( 'NONE',  ( -2.264806262022998062, 0.000000000000000000, -14.82803603298499340 ) ) ;
#9201 = CARTESIAN_POINT ( 'NONE',  ( 7.500000000000003553, 0.000000000000000000, 13.39999999999999858 ) ) ;
#9202 = LINE ( 'NONE', #5967, #9317 ) ;
#9203 = VERTEX_POINT ( 'NONE', #13178 ) ;
#9204 = ADVANCED_FACE ( 'NONE', ( #6020 ), #9947, .F. ) ;
#9205 = LINE ( 'NONE', #4110, #8608 ) ;
#9206 = CARTESIAN_POINT ( 'NONE',  ( 12.25836857253663581, 3.000000000000000000, 5.784789447945493990 ) ) ;
#9207 = ORIENTED_EDGE ( 'NONE', *, *, #2374, .T. ) ;
#9208 = CARTESIAN_POINT ( 'NONE',  ( -11.70905276178463872, 0.000000000000000000, -9.375397774054366806 ) ) ;
#9209 = DIRECTION ( 'NONE',  ( 0.8355447872852816982, 4.667094087487695270E-23, 0.5494223406819142008 ) ) ;
#9210 = CYLINDRICAL_SURFACE ( 'NONE', #6397, 14.25000000000000178 ) ;
#9211 = FACE_OUTER_BOUND ( 'NONE', #8517, .T. ) ;
#9212 = EDGE_CURVE ( 'NONE', #9002, #8355, #12599, .T. ) ;
#9213 = CARTESIAN_POINT ( 'NONE',  ( -14.16466328168010769, 3.000000000000000000, -1.557181465540673271 ) ) ;
#9214 = CARTESIAN_POINT ( 'NONE',  ( -8.158651161643904359, 3.000000000000000000, -8.922136023539605887 ) ) ;
#9215 = CARTESIAN_POINT ( 'NONE',  ( 30.79786191028635400, 3.000000000000000000, -6.999232361977355765 ) ) ;
#9216 = ORIENTED_EDGE ( 'NONE', *, *, #12533, .T. ) ;
#9217 = CARTESIAN_POINT ( 'NONE',  ( 6.079397157347990799, 0.000000000000000000, 5.110946565852551693 ) ) ;
#9218 = ORIENTED_EDGE ( 'NONE', *, *, #1829, .T. ) ;
#9219 = ORIENTED_EDGE ( 'NONE', *, *, #6599, .T. ) ;
#9220 = CARTESIAN_POINT ( 'NONE',  ( -14.90895795148411374, 3.000000000000000000, -1.650143266773683726 ) ) ;
#9221 = VECTOR ( 'NONE', #12194, 1000.000000000000000 ) ;
#9222 = ORIENTED_EDGE ( 'NONE', *, *, #10057, .F. ) ;
#9223 = B_SPLINE_CURVE_WITH_KNOTS ( 'NONE', 3,
 ( #12777, #1267, #6634, #1330 ),
 .UNSPECIFIED., .F., .F.,
 ( 4, 4 ),
 ( 0.1276832474596256706, 1.000000000000000000 ),
 .UNSPECIFIED. ) ;
#9224 = DIRECTION ( 'NONE',  ( -0.000000000000000000, -1.000000000000000000, -0.000000000000000000 ) ) ;
#9225 = SURFACE_STYLE_USAGE ( .BOTH. , #901 ) ;
#9226 = CARTESIAN_POINT ( 'NONE',  ( 7.151505841916629080, 9.000000000000000000, 1.752496229622501511 ) ) ;
#9227 = CYLINDRICAL_SURFACE ( 'NONE', #13061, 3.000000000000000000 ) ;
#9228 = VECTOR ( 'NONE', #12781, 1000.000000000000000 ) ;
#9229 = DIRECTION ( 'NONE',  ( 0.000000000000000000, 1.000000000000000000, 0.000000000000000000 ) ) ;
#9230 = VECTOR ( 'NONE', #7523, 1000.000000000000000 ) ;
#9231 = CARTESIAN_POINT ( 'NONE',  ( 2.264806262022877714, 3.000000000000000000, -14.82803603298501471 ) ) ;
#9232 = EDGE_LOOP ( 'NONE', ( #10440, #2010, #4484, #3119 ) ) ;
#9233 = LINE ( 'NONE', #13383, #2928 ) ;
#9234 = EDGE_LOOP ( 'NONE', ( #342, #7368, #4688, #11518 ) ) ;
#9235 = EDGE_LOOP ( 'NONE', ( #10263, #10153, #12019, #4774 ) ) ;
#9236 = DIRECTION ( 'NONE',  ( -0.000000000000000000, -1.000000000000000000, -0.000000000000000000 ) ) ;
#9237 = EDGE_LOOP ( 'NONE', ( #10101, #4503, #3121, #3632, #96, #11607, #4647, #4552, #8795, #11695, #13034, #3372, #13554, #12985, #10953, #9083, #13585, #5659, #10266, #11406, #11207, #8930, #8294, #10158, #6944, #4821, #557, #4224, #6795, #861, #12876, #4002, #5507, #9926, #10872, #11159, #3677, #1696, #10817, #6880, #6192, #1245, #161, #8490, #7661, #4349, #2303, #13107, #12518, #160, #10195, #11144, #13570, #6752 ) ) ;
#9238 = AXIS2_PLACEMENT_3D ( 'NONE', #9245, #13462, #6220 ) ;
#9239 = AXIS2_PLACEMENT_3D ( 'NONE', #11435, #2004, #11236 ) ;
#9240 = ADVANCED_FACE ( 'NONE', ( #4985 ), #10503, .T. ) ;
#9241 = DIRECTION ( 'NONE',  ( 0.000000000000000000, 1.000000000000000000, -0.000000000000000000 ) ) ;
#9242 = DIRECTION ( 'NONE',  ( 1.000000000000000000, 0.000000000000000000, -1.055752450943286467E-16 ) ) ;
#9243 = CARTESIAN_POINT ( 'NONE',  ( -11.80612203322752585, 0.000000000000000000, 2.604531154829235362 ) ) ;
#9244 = LINE ( 'NONE', #13532, #4176 ) ;
#9245 = CARTESIAN_POINT ( 'NONE',  ( 31.00000000000000000, 0.09999999999999982514, 0.000000000000000000 ) ) ;
#9246 = DIRECTION ( 'NONE',  ( 0.000000000000000000, 0.000000000000000000, 1.000000000000000000 ) ) ;
#9247 = CARTESIAN_POINT ( 'NONE',  ( -1.650143266773857142, 3.000000000000000000, -14.90895795148409952 ) ) ;
#9248 = FACE_OUTER_BOUND ( 'NONE', #12245, .T. ) ;
#9249 = ORIENTED_EDGE ( 'NONE', *, *, #3468, .T. ) ;
#9250 = CARTESIAN_POINT ( 'NONE',  ( -9.573149624528719315, 3.000000000000000000, -8.795158114916407754 ) ) ;
#9251 = VECTOR ( 'NONE', #5980, 1000.000000000000000 ) ;
#9252 = VECTOR ( 'NONE', #3636, 1000.000000000000000 ) ;
#9253 = ORIENTED_EDGE ( 'NONE', *, *, #6920, .F. ) ;
#9254 = B_SPLINE_CURVE_WITH_KNOTS ( 'NONE', 3,
 ( #3545, #10925, #1562, #2452 ),
 .UNSPECIFIED., .F., .F.,
 ( 4, 4 ),
 ( 0.1547128134717859205, 1.000000000000000000 ),
 .UNSPECIFIED. ) ;
#9255 = ORIENTED_EDGE ( 'NONE', *, *, #12656, .F. ) ;
#9256 = VERTEX_POINT ( 'NONE', #4087 ) ;
#9257 = EDGE_CURVE ( 'NONE', #3224, #10361, #8288, .T. ) ;
#9258 = EDGE_CURVE ( 'NONE', #2349, #5599, #8213, .T. ) ;
#9259 = ORIENTED_EDGE ( 'NONE', *, *, #6812, .T. ) ;
#9260 = DIRECTION ( 'NONE',  ( 0.000000000000000000, 1.000000000000000000, 0.000000000000000000 ) ) ;
#9261 = EDGE_CURVE ( 'NONE', #7435, #6099, #12634, .T. ) ;
#9262 = CARTESIAN_POINT ( 'NONE',  ( 10.14701493152832512, 3.000000000000000000, -29.73855628788322747 ) ) ;
#9263 = AXIS2_PLACEMENT_3D ( 'NONE', #3206, #3067, #3009 ) ;
#9264 = AXIS2_PLACEMENT_3D ( 'NONE', #4105, #1213, #6169 ) ;
#9265 = FACE_OUTER_BOUND ( 'NONE', #9290, .T. ) ;
#9266 = EDGE_CURVE ( 'NONE', #7795, #12927, #9123, .T. ) ;
#9267 = DIRECTION ( 'NONE',  ( 0.000000000000000000, 0.000000000000000000, 1.000000000000000000 ) ) ;
#9268 = CARTESIAN_POINT ( 'NONE',  ( 8.430890348300565051, 0.000000000000000000, -11.48836750521728334 ) ) ;
#9269 = DIRECTION ( 'NONE',  ( 0.000000000000000000, 0.000000000000000000, 1.000000000000000000 ) ) ;
#9270 = FACE_OUTER_BOUND ( 'NONE', #8911, .T. ) ;
#9271 = ORIENTED_EDGE ( 'NONE', *, *, #7510, .T. ) ;
#9272 = VECTOR ( 'NONE', #10900, 1000.000000000000227 ) ;
#9273 = CARTESIAN_POINT ( 'NONE',  ( 0.000000000000000000, 9.000000000000000000, 0.000000000000000000 ) ) ;
#9274 = CARTESIAN_POINT ( 'NONE',  ( 0.000000000000000000, 9.000000000000000000, 0.000000000000000000 ) ) ;
#9275 = EDGE_CURVE ( 'NONE', #13474, #8960, #10446, .T. ) ;
#9276 = VERTEX_POINT ( 'NONE', #1896 ) ;
#9277 = B_SPLINE_CURVE_WITH_KNOTS ( 'NONE', 3,
 ( #6811, #6964, #13223, #7103 ),
 .UNSPECIFIED., .F., .F.,
 ( 4, 4 ),
 ( 0.000000000000000000, 0.8724294488011768989 ),
 .UNSPECIFIED. ) ;
#9278 = CARTESIAN_POINT ( 'NONE',  ( -8.222660081691577361, 3.000000000000000000, -8.549999999999998934 ) ) ;
#9279 = CIRCLE ( 'NONE', #491, 0.7499999999999997780 ) ;
#9280 = EDGE_CURVE ( 'NONE', #7515, #5524, #5495, .T. ) ;
#9281 =( NAMED_UNIT ( * ) PLANE_ANGLE_UNIT ( ) SI_UNIT ( $, .RADIAN. ) );
#9282 = EDGE_CURVE ( 'NONE', #3238, #10250, #493, .T. ) ;
#9283 = AXIS2_PLACEMENT_3D ( 'NONE', #3467, #6641, #7617 ) ;
#9284 = LINE ( 'NONE', #6182, #10794 ) ;
#9285 = DIRECTION ( 'NONE',  ( 0.000000000000000000, 0.000000000000000000, 1.000000000000000000 ) ) ;
#9286 = CARTESIAN_POINT ( 'NONE',  ( -9.593885948927676210, 0.000000000000000000, 8.504652361247165615 ) ) ;
#9287 = CARTESIAN_POINT ( 'NONE',  ( -6.524296280129988190, 0.000000000000000000, -3.413039245436654490 ) ) ;
#9288 = B_SPLINE_CURVE_WITH_KNOTS ( 'NONE', 3,
 ( #1393, #228, #10632, #7720 ),
 .UNSPECIFIED., .F., .F.,
 ( 4, 4 ),
 ( 0.000000000000000000, 0.5855695330273008592 ),
 .UNSPECIFIED. ) ;
#9289 = CARTESIAN_POINT ( 'NONE',  ( 6.079397157347990799, 9.000000000000000000, 5.110946565852551693 ) ) ;
#9290 = EDGE_LOOP ( 'NONE', ( #2835, #5424, #135, #2000 ) ) ;
#9291 = UNCERTAINTY_MEASURE_WITH_UNIT (LENGTH_MEASURE( 1.000000000000000082E-05 ), #11929, 'distance_accuracy_value', 'NONE');
#9292 = CIRCLE ( 'NONE', #6214, 12.08999999999737440 ) ;
#9293 = ORIENTED_EDGE ( 'NONE', *, *, #12054, .F. ) ;
#9294 = CARTESIAN_POINT ( 'NONE',  ( 26.30958424017656938, 0.000000000000000000, 4.500000000000000888 ) ) ;
#9295 = VECTOR ( 'NONE', #1616, 1000.000000000000000 ) ;
#9296 = VECTOR ( 'NONE', #8487, 1000.000000000000000 ) ;
#9297 = ORIENTED_EDGE ( 'NONE', *, *, #3657, .T. ) ;
#9298 = DIRECTION ( 'NONE',  ( 0.000000000000000000, 0.000000000000000000, 1.000000000000000000 ) ) ;
#9299 =( NAMED_UNIT ( * ) PLANE_ANGLE_UNIT ( ) SI_UNIT ( $, .RADIAN. ) );
#9300 = CARTESIAN_POINT ( 'NONE',  ( 8.373678438139048552, 9.000000000000000000, 1.459968977288628178 ) ) ;
#9301 = CIRCLE ( 'NONE', #6667, 3.100000000000000533 ) ;
#9302 = FACE_OUTER_BOUND ( 'NONE', #12664, .T. ) ;
#9303 = CIRCLE ( 'NONE', #6444, 6.750000000000000888 ) ;
#9304 = VECTOR ( 'NONE', #5501, 1000.000000000000000 ) ;
#9305 = CARTESIAN_POINT ( 'NONE',  ( -12.68816982652970893, 3.000000000000000000, 2.830255545554337004 ) ) ;
#9306 = CARTESIAN_POINT ( 'NONE',  ( -4.072642252455976219, 0.000000000000000000, -12.14623037080101398 ) ) ;
#9307 = VERTEX_POINT ( 'NONE', #11526 ) ;
#9308 = DIRECTION ( 'NONE',  ( -0.000000000000000000, -1.000000000000000000, -0.000000000000000000 ) ) ;
#9309 = EDGE_LOOP ( 'NONE', ( #12021, #5662, #6260, #7211 ) ) ;
#9310 = ORIENTED_EDGE ( 'NONE', *, *, #9812, .T. ) ;
#9311 = CARTESIAN_POINT ( 'NONE',  ( -6.025412986832177076, 0.000000000000000000, -13.73660796332610268 ) ) ;
#9312 = EDGE_CURVE ( 'NONE', #10532, #11648, #7196, .T. ) ;
#9313 = EDGE_CURVE ( 'NONE', #4866, #10838, #2383, .T. ) ;
#9314 = ORIENTED_EDGE ( 'NONE', *, *, #4556, .T. ) ;
#9315 = AXIS2_PLACEMENT_3D ( 'NONE', #1694, #802, #4991 ) ;
#9316 = CIRCLE ( 'NONE', #4247, 6.750000000000000888 ) ;
#9317 = VECTOR ( 'NONE', #3897, 1000.000000000000000 ) ;
#9318 = AXIS2_PLACEMENT_3D ( 'NONE', #4616, #4824, #8950 ) ;
#9319 = B_SPLINE_CURVE_WITH_KNOTS ( 'NONE', 3,
 ( #1812, #8074, #638, #6009 ),
 .UNSPECIFIED., .F., .F.,
 ( 4, 4 ),
 ( 0.1547128134717859205, 1.000000000000000000 ),
 .UNSPECIFIED. ) ;
#9320 = CARTESIAN_POINT ( 'NONE',  ( 8.504652361247167391, 0.000000000000000000, 9.593885948927674434 ) ) ;
#9321 = SURFACE_STYLE_FILL_AREA ( #13331 ) ;
#9322 = CARTESIAN_POINT ( 'NONE',  ( 2.458659560121117416, 0.000000000000000000, -8.136645080586040635 ) ) ;
#9323 = DIRECTION ( 'NONE',  ( -0.000000000000000000, -1.000000000000000000, -0.000000000000000000 ) ) ;
#9324 = CARTESIAN_POINT ( 'NONE',  ( 0.000000000000000000, 3.000000000000000000, 0.000000000000000000 ) ) ;
#9325 = CARTESIAN_POINT ( 'NONE',  ( -11.52662650599092409, 0.000000000000000000, 3.647599401157420651 ) ) ;
#9326 = CARTESIAN_POINT ( 'NONE',  ( -9.375397774054503586, 3.000000000000000000, -11.70905276178452503 ) ) ;
#9327 = CARTESIAN_POINT ( 'NONE',  ( -0.8123631076467130452, 1.734723475976807094E-15, -6.700937709107178009 ) ) ;
#9328 = CARTESIAN_POINT ( 'NONE',  ( -11.70905276178463872, 3.000000000000000000, -9.375397774054366806 ) ) ;
#9329 = CIRCLE ( 'NONE', #5800, 8.500000000000000000 ) ;
#9330 = ORIENTED_EDGE ( 'NONE', *, *, #10350, .F. ) ;
#9331 = CARTESIAN_POINT ( 'NONE',  ( -5.999999999999991118, 3.000000000000000000, 28.50000000000000000 ) ) ;
#9332 = CIRCLE ( 'NONE', #3378, 2.999999999999999112 ) ;
#9333 = ORIENTED_EDGE ( 'NONE', *, *, #11824, .F. ) ;
#9334 = ORIENTED_EDGE ( 'NONE', *, *, #1366, .T. ) ;
#9335 = ORIENTED_EDGE ( 'NONE', *, *, #10543, .F. ) ;
#9336 = VERTEX_POINT ( 'NONE', #10425 ) ;
#9337 = DIRECTION ( 'NONE',  ( -0.000000000000000000, -1.000000000000000000, -0.000000000000000000 ) ) ;
#9338 = AXIS2_PLACEMENT_3D ( 'NONE', #3896, #12323, #9269 ) ;
#9339 = CIRCLE ( 'NONE', #4053, 1.000000000000000888 ) ;
#9340 =( NAMED_UNIT ( * ) PLANE_ANGLE_UNIT ( ) SI_UNIT ( $, .RADIAN. ) );
#9341 = CARTESIAN_POINT ( 'NONE',  ( 0.000000000000000000, 1.000000000000000000, 0.000000000000000000 ) ) ;
#9342 = CARTESIAN_POINT ( 'NONE',  ( 2.719999999999997087, 2.000000000000000000, -7.500000000000000000 ) ) ;
#9343 = CARTESIAN_POINT ( 'NONE',  ( -7.065816209474154341, 3.000000000000000000, 10.69794375946289833 ) ) ;
#9344 = DIRECTION ( 'NONE',  ( 0.000000000000000000, 1.000000000000000000, -0.000000000000000000 ) ) ;
#9345 = EDGE_CURVE ( 'NONE', #9927, #10341, #5330, .T. ) ;
#9347 = CIRCLE ( 'NONE', #8891, 12.08999999999737263 ) ;
#9346 = PRODUCT_RELATED_PRODUCT_CATEGORY ( 'part', '', ( #528 ) ) ;
#9348 = DIRECTION ( 'NONE',  ( 0.000000000000000000, 1.000000000000000000, -0.000000000000000000 ) ) ;
#9349 = AXIS2_PLACEMENT_3D ( 'NONE', #10275, #8468, #5102 ) ;
#9350 = VERTEX_POINT ( 'NONE', #11393 ) ;
#9351 = B_SPLINE_CURVE_WITH_KNOTS ( 'NONE', 3,
 ( #11326, #1895, #2988, #6984 ),
 .UNSPECIFIED., .F., .F.,
 ( 4, 4 ),
 ( 0.000000000000000000, 0.5855695330273008592 ),
 .UNSPECIFIED. ) ;
#9352 = CARTESIAN_POINT ( 'NONE',  ( 0.000000000000000000, 0.09999999999999982514, 0.000000000000000000 ) ) ;
#9353 = FACE_OUTER_BOUND ( 'NONE', #10853, .T. ) ;
#9354 = ORIENTED_EDGE ( 'NONE', *, *, #5934, .F. ) ;
#9355 = CARTESIAN_POINT ( 'NONE',  ( -5.299649803506881085, 9.000000000000000000, -6.645578376649351249 ) ) ;
#9356 = B_SPLINE_CURVE_WITH_KNOTS ( 'NONE', 3,
 ( #2262, #11776, #13573, #4129 ),
 .UNSPECIFIED., .F., .F.,
 ( 4, 4 ),
 ( 0.9090903094065657664, 0.9385083864668765097 ),
 .UNSPECIFIED. ) ;
#9357 = CARTESIAN_POINT ( 'NONE',  ( 31.00000000000000000, 2.900000000000000355, 0.000000000000000000 ) ) ;
#9358 = COLOUR_RGB ( '',0.7803921568627451011, 0.7607843137254901578, 0.7411764705882353255 ) ;
#9359 =( NAMED_UNIT ( * ) SI_UNIT ( $, .STERADIAN. ) SOLID_ANGLE_UNIT ( ) );
#9360 = VECTOR ( 'NONE', #5436, 1000.000000000000000 ) ;
#9361 = CARTESIAN_POINT ( 'NONE',  ( -8.100301009650792139, 9.000000000000000000, -2.575873357339267589 ) ) ;
#9362 = CYLINDRICAL_SURFACE ( 'NONE', #8579, 1.500000000000000666 ) ;
#9363 = DIRECTION ( 'NONE',  ( -0.000000000000000000, -1.000000000000000000, 0.000000000000000000 ) ) ;
#9364 = EDGE_CURVE ( 'NONE', #4139, #9908, #991, .T. ) ;
#9365 = CYLINDRICAL_SURFACE ( 'NONE', #6495, 5.000000000000000000 ) ;
#9366 = EDGE_CURVE ( 'NONE', #7638, #12626, #8189, .T. ) ;
#9367 = CARTESIAN_POINT ( 'NONE',  ( -8.922226997226891498, 0.000000000000000000, -8.158551673544284455 ) ) ;
#9368 = ORIENTED_EDGE ( 'NONE', *, *, #13274, .F. ) ;
#9369 = ORIENTED_EDGE ( 'NONE', *, *, #3703, .T. ) ;
#9370 = EDGE_CURVE ( 'NONE', #4457, #9614, #10223, .T. ) ;
#9371 = ORIENTED_EDGE ( 'NONE', *, *, #5171, .T. ) ;
#9372 = DIRECTION ( 'NONE',  ( 0.000000000000000000, 0.000000000000000000, -1.000000000000000000 ) ) ;
#9373 = EDGE_CURVE ( 'NONE', #8874, #2998, #406, .T. ) ;
#9374 = ORIENTED_EDGE ( 'NONE', *, *, #8204, .T. ) ;
#9375 = DIRECTION ( 'NONE',  ( 0.000000000000000000, 1.000000000000000000, -0.000000000000000000 ) ) ;
#9376 = CARTESIAN_POINT ( 'NONE',  ( -1.650143266773857142, 0.000000000000000000, -14.90895795148409952 ) ) ;
#9377 = CARTESIAN_POINT ( 'NONE',  ( -2.976187484161006314, 9.000000000000000000, 7.363908159724035229 ) ) ;
#9378 = AXIS2_PLACEMENT_3D ( 'NONE', #4807, #8994, #5908 ) ;
#9379 = DIRECTION ( 'NONE',  ( -0.000000000000000000, -1.000000000000000000, -0.000000000000000000 ) ) ;
#9380 = ADVANCED_FACE ( 'NONE', ( #12761 ), #10696, .F. ) ;
#9381 = DIRECTION ( 'NONE',  ( 1.000000000000000000, 0.000000000000000000, 0.000000000000000000 ) ) ;
#9382 = CARTESIAN_POINT ( 'NONE',  ( -12.25836857253663759, 0.000000000000000000, -5.784789447945487773 ) ) ;
#9383 = ORIENTED_EDGE ( 'NONE', *, *, #1445, .F. ) ;
#9384 = LINE ( 'NONE', #7188, #5129 ) ;
#9385 = ORIENTED_EDGE ( 'NONE', *, *, #6244, .F. ) ;
#9386 = ORIENTED_EDGE ( 'NONE', *, *, #10627, .T. ) ;
#9387 = CARTESIAN_POINT ( 'NONE',  ( -4.227250083625790467, 3.000000000000000000, -13.17831234185026013 ) ) ;
#9388 = EDGE_CURVE ( 'NONE', #13098, #4297, #12960, .T. ) ;
#9389 = ORIENTED_EDGE ( 'NONE', *, *, #8252, .F. ) ;
#9390 = DIRECTION ( 'NONE',  ( -0.000000000000000000, -1.000000000000000000, -0.000000000000000000 ) ) ;
#9391 = DIRECTION ( 'NONE',  ( -0.000000000000000000, -1.000000000000000000, -0.000000000000000000 ) ) ;
#9392 = CARTESIAN_POINT ( 'NONE',  ( 2.394769219159762930, 9.000000000000000000, -6.310909632292713844 ) ) ;
#9393 = CARTESIAN_POINT ( 'NONE',  ( 40.92955321648837241, 3.000000000000000000, -6.070049343411170639 ) ) ;
#9394 = CARTESIAN_POINT ( 'NONE',  ( -12.78643498603817896, 3.000000000000000000, 0.7901945867173603144 ) ) ;
#9395 = DIRECTION ( 'NONE',  ( 0.000000000000000000, 0.000000000000000000, 1.000000000000000000 ) ) ;
#9396 = ADVANCED_FACE ( 'NONE', ( #3382 ), #4355, .F. ) ;
#9397 = DIRECTION ( 'NONE',  ( -0.000000000000000000, -1.000000000000000000, -0.000000000000000000 ) ) ;
#9398 = EDGE_CURVE ( 'NONE', #2521, #10261, #10827, .T. ) ;
#9399 = CARTESIAN_POINT ( 'NONE',  ( 0.000000000000000000, 3.000000000000000000, -1.500000000000000000 ) ) ;
#9400 = VERTEX_POINT ( 'NONE', #3310 ) ;
#9401 = FACE_BOUND ( 'NONE', #13419, .T. ) ;
#9402 = ORIENTED_EDGE ( 'NONE', *, *, #6575, .T. ) ;
#9403 = ORIENTED_EDGE ( 'NONE', *, *, #5665, .T. ) ;
#9404 = ORIENTED_EDGE ( 'NONE', *, *, #11841, .T. ) ;
#9405 = EDGE_LOOP ( 'NONE', ( #4867, #1233, #3469, #12144 ) ) ;
#9406 = LINE ( 'NONE', #7338, #11740 ) ;
#9407 = SURFACE_STYLE_USAGE ( .BOTH. , #4231 ) ;
#9408 = CARTESIAN_POINT ( 'NONE',  ( 12.63269908545826503, 3.000000000000000000, -5.340493616518843467 ) ) ;
#9409 = DIRECTION ( 'NONE',  ( -0.000000000000000000, -1.000000000000000000, -0.000000000000000000 ) ) ;
#9410 = CARTESIAN_POINT ( 'NONE',  ( 26.30958424017656938, 3.000000000000000000, 1.399999999999999911 ) ) ;
#9411 = ORIENTED_EDGE ( 'NONE', *, *, #5562, .T. ) ;
#9412 = LINE ( 'NONE', #6176, #1587 ) ;
#9413 = CYLINDRICAL_SURFACE ( 'NONE', #10626, 14.25000000000000178 ) ;
#9414 = ORIENTED_EDGE ( 'NONE', *, *, #3292, .T. ) ;
#9415 = CARTESIAN_POINT ( 'NONE',  ( -11.48836750521728867, 0.000000000000000000, -8.430890348300557946 ) ) ;
#9416 = EDGE_CURVE ( 'NONE', #13159, #732, #2358, .T. ) ;
#9417 = FACE_OUTER_BOUND ( 'NONE', #10796, .T. ) ;
#9418 = APPLICATION_PROTOCOL_DEFINITION ( 'draft international standard', 'automotive_design', 1998, #9850 ) ;
#9419 = LINE ( 'NONE', #12537, #12367 ) ;
#9420 = LINE ( 'NONE', #887, #7061 ) ;
#9421 = CARTESIAN_POINT ( 'NONE',  ( 2.999999999999995559, 2.000000000000000000, -10.00000000000000355 ) ) ;
#9422 = DIRECTION ( 'NONE',  ( 0.000000000000000000, 0.000000000000000000, 1.000000000000000000 ) ) ;
#9423 = FACE_BOUND ( 'NONE', #12544, .T. ) ;
#9424 = ORIENTED_EDGE ( 'NONE', *, *, #2232, .F. ) ;
#9425 = ORIENTED_EDGE ( 'NONE', *, *, #7611, .F. ) ;
#9426 = CARTESIAN_POINT ( 'NONE',  ( -0.5501230721523990841, 0.000000000000000000, -12.98835496148299384 ) ) ;
#9427 = ORIENTED_EDGE ( 'NONE', *, *, #10118, .F. ) ;
#9428 = EDGE_CURVE ( 'NONE', #10734, #5027, #716, .T. ) ;
#9429 = EDGE_CURVE ( 'NONE', #12875, #344, #2246, .T. ) ;
#9430 = B_SPLINE_CURVE_WITH_KNOTS ( 'NONE', 3,
 ( #11506, #12286, #3993, #2003 ),
 .UNSPECIFIED., .F., .F.,
 ( 4, 4 ),
 ( 0.000000000000000000, 0.8452273900860258760 ),
 .UNSPECIFIED. ) ;
#9431 = DIRECTION ( 'NONE',  ( -0.000000000000000000, -1.000000000000000000, -0.000000000000000000 ) ) ;
#9432 = CARTESIAN_POINT ( 'NONE',  ( -14.20034848914871795, 3.000000000000000000, 2.631756770590945482 ) ) ;
#9433 = DIRECTION ( 'NONE',  ( 0.000000000000000000, 0.000000000000000000, 1.000000000000000000 ) ) ;
#9434 = CARTESIAN_POINT ( 'NONE',  ( 0.6724118135762067183, 3.000000000000000000, -13.82336506795094344 ) ) ;
#9435 = EDGE_CURVE ( 'NONE', #2998, #5225, #9288, .T. ) ;
#9436 = LINE ( 'NONE', #15, #9496 ) ;
#9437 = CARTESIAN_POINT ( 'NONE',  ( -13.97385902380755240, 0.000000000000000000, -5.452638258930474713 ) ) ;
#9438 = ORIENTED_EDGE ( 'NONE', *, *, #3473, .F. ) ;
#9439 = CARTESIAN_POINT ( 'NONE',  ( -8.158551673544545579, 3.000000000000000000, 8.922226997226644585 ) ) ;
#9440 = ORIENTED_EDGE ( 'NONE', *, *, #11841, .F. ) ;
#9441 = ORIENTED_EDGE ( 'NONE', *, *, #1569, .T. ) ;
#9442 = CARTESIAN_POINT ( 'NONE',  ( -5.452638258930639914, 0.000000000000000000, -13.97385902380748313 ) ) ;
#9443 = VERTEX_POINT ( 'NONE', #9652 ) ;
#9444 = EDGE_CURVE ( 'NONE', #11926, #6767, #297, .T. ) ;
#9445 = CARTESIAN_POINT ( 'NONE',  ( 0.000000000000000000, 0.000000000000000000, 0.000000000000000000 ) ) ;
#9446 = CARTESIAN_POINT ( 'NONE',  ( 9.573149624528804580, 0.000000000000000000, -8.795158114916638681 ) ) ;
#9447 = CARTESIAN_POINT ( 'NONE',  ( 4.690415759823430619, 3.000000000000000000, -1.500000000000000000 ) ) ;
#9448 = CARTESIAN_POINT ( 'NONE',  ( 12.00000000000000178, 1.999999999999993117, 10.00000000000000000 ) ) ;
#9449 = CIRCLE ( 'NONE', #6363, 12.08999999999737085 ) ;
#9450 = DIRECTION ( 'NONE',  ( 0.000000000000000000, 0.000000000000000000, 1.000000000000000000 ) ) ;
#9451 = LINE ( 'NONE', #856, #8641 ) ;
#9452 = EDGE_CURVE ( 'NONE', #10694, #5785, #2211, .T. ) ;
#9453 = CARTESIAN_POINT ( 'NONE',  ( -4.340891659662447388, 9.000000000000000000, 6.651128039276029469 ) ) ;
#9454 = CARTESIAN_POINT ( 'NONE',  ( -6.506620931068619385, 0.000000000000000000, -10.18979803820057306 ) ) ;
#9455 = ORIENTED_EDGE ( 'NONE', *, *, #1183, .T. ) ;
#9456 = CARTESIAN_POINT ( 'NONE',  ( 17.00000000000000355, 0.000000000000000000, -14.92471123914605435 ) ) ;
#9457 = VERTEX_POINT ( 'NONE', #9787 ) ;
#9458 = EDGE_LOOP ( 'NONE', ( #6996, #11241 ) ) ;
#9459 = VECTOR ( 'NONE', #7198, 1000.000000000000000 ) ;
#9460 = VECTOR ( 'NONE', #1897, 1000.000000000000000 ) ;
#9461 = VERTEX_POINT ( 'NONE', #8744 ) ;
#9462 = ADVANCED_FACE ( 'NONE', ( #6556 ), #10840, .T. ) ;
#9463 = EDGE_CURVE ( 'NONE', #3023, #12683, #7521, .T. ) ;
#9464 = VERTEX_POINT ( 'NONE', #10756 ) ;
#9465 = FACE_OUTER_BOUND ( 'NONE', #10435, .T. ) ;
#9466 = CARTESIAN_POINT ( 'NONE',  ( 7.500000000000004441, 3.000000000000000000, 21.89999999999999858 ) ) ;
#9467 = DIRECTION ( 'NONE',  ( 0.000000000000000000, 0.000000000000000000, -1.000000000000000000 ) ) ;
#9468 = VECTOR ( 'NONE', #1989, 1000.000000000000000 ) ;
#9469 = CARTESIAN_POINT ( 'NONE',  ( 8.093005444143644311, 0.000000000000000000, -2.598704077239528232 ) ) ;
#9470 = CARTESIAN_POINT ( 'NONE',  ( 2.719999999999997087, 2.000000000000000000, -4.500000000000000888 ) ) ;
#9471 = AXIS2_PLACEMENT_3D ( 'NONE', #11777, #10740, #3429 ) ;
#9472 = CARTESIAN_POINT ( 'NONE',  ( -8.504652361247167391, 3.000000000000000000, -9.593885948927674434 ) ) ;
#9473 = VERTEX_POINT ( 'NONE', #9523 ) ;
#9474 = ORIENTED_EDGE ( 'NONE', *, *, #2145, .T. ) ;
#9475 = LINE ( 'NONE', #9616, #3778 ) ;
#9476 = VECTOR ( 'NONE', #7344, 1000.000000000000000 ) ;
#9477 = VECTOR ( 'NONE', #679, 1000.000000000000000 ) ;
#9478 = EDGE_CURVE ( 'NONE', #2426, #2659, #9717, .T. ) ;
#9479 = VERTEX_POINT ( 'NONE', #1319 ) ;
#9480 = DIRECTION ( 'NONE',  ( 0.000000000000000000, 1.000000000000000000, 0.000000000000000000 ) ) ;
#9481 = CARTESIAN_POINT ( 'NONE',  ( 0.000000000000000000, 9.000000000000000000, -0.4000000000000000222 ) ) ;
#9482 =( LENGTH_UNIT ( ) NAMED_UNIT ( * ) SI_UNIT ( .MILLI., .METRE. ) );
#9483 = FACE_OUTER_BOUND ( 'NONE', #8621, .T. ) ;
#9484 = CARTESIAN_POINT ( 'NONE',  ( -3.647470871583628593, 3.000000000000000000, 11.52666717836884125 ) ) ;
#9485 = DIRECTION ( 'NONE',  ( 0.000000000000000000, 0.000000000000000000, 1.000000000000000000 ) ) ;
#9486 = CIRCLE ( 'NONE', #9924, 1.499999999999998668 ) ;
#9487 = DIRECTION ( 'NONE',  ( -0.7772490812545752581, 0.000000000000000000, -0.6291930273683257191 ) ) ;
#9488 = PLANE ( 'NONE',  #11524 ) ;
#9489 = ORIENTED_EDGE ( 'NONE', *, *, #8339, .F. ) ;
#9490 = EDGE_CURVE ( 'NONE', #7533, #4645, #3344, .T. ) ;
#9491 = ORIENTED_EDGE ( 'NONE', *, *, #8319, .T. ) ;
#9492 = ORIENTED_EDGE ( 'NONE', *, *, #6836, .T. ) ;
#9493 = CARTESIAN_POINT ( 'NONE',  ( 12.00000000000000533, 2.749999999999990230, 10.00000000000000178 ) ) ;
#9494 = EDGE_LOOP ( 'NONE', ( #11774, #7063, #5455, #3871 ) ) ;
#9495 = CIRCLE ( 'NONE', #12153, 13.50000000000000178 ) ;
#9496 = VECTOR ( 'NONE', #1942, 1000.000000000000000 ) ;
#9497 = CARTESIAN_POINT ( 'NONE',  ( -6.515098946627274401, 9.000000000000000000, 3.430563300314522390 ) ) ;
#9498 = FILL_AREA_STYLE_COLOUR ( '', #10897 ) ;
#9499 = B_SPLINE_SURFACE_WITH_KNOTS ( 'NONE', 3, 1, ( 
 ( #7116, #8326 ),
 ( #12553, #6134 ),
 ( #3096, #12289 ),
 ( #13517, #7185 ) ),
 .UNSPECIFIED., .F., .F., .F.,
 ( 4, 4 ),
 ( 2, 2 ),
 ( 0.000000000000000000, 0.5855695330273008592 ),
 ( 0.000000000000000000, 1.000000000000000000 ),
 .UNSPECIFIED. ) ;
#9500 = CARTESIAN_POINT ( 'NONE',  ( -7.500000000000000000, 3.000000000000000000, -1.500000000000000666 ) ) ;
#9501 = CARTESIAN_POINT ( 'NONE',  ( 0.000000000000000000, 3.000000000000000000, 0.000000000000000000 ) ) ;
#9502 = DIRECTION ( 'NONE',  ( 0.000000000000000000, 0.000000000000000000, 1.000000000000000000 ) ) ;
#9503 = LINE ( 'NONE', #9000, #8610 ) ;
#9504 = CARTESIAN_POINT ( 'NONE',  ( -13.61374091949023679, 0.000000000000000000, -4.821006024660923650 ) ) ;
#9505 = ORIENTED_EDGE ( 'NONE', *, *, #1875, .T. ) ;
#9506 = CIRCLE ( 'NONE', #3560, 1.499999999999998668 ) ;
#9507 = LINE ( 'NONE', #11850, #10411 ) ;
#9508 = ORIENTED_EDGE ( 'NONE', *, *, #1049, .T. ) ;
#9509 = VECTOR ( 'NONE', #5944, 1000.000000000000114 ) ;
#9510 = CIRCLE ( 'NONE', #10605, 0.09999999999999982514 ) ;
#9511 = ORIENTED_EDGE ( 'NONE', *, *, #681, .F. ) ;
#9512 = EDGE_CURVE ( 'NONE', #10283, #291, #3447, .T. ) ;
#9513 = EDGE_CURVE ( 'NONE', #12626, #11577, #13166, .T. ) ;
#9514 = ORIENTED_EDGE ( 'NONE', *, *, #7922, .F. ) ;
#9515 = CARTESIAN_POINT ( 'NONE',  ( 5.958322434183388694, 9.000000000000000000, -6.062045345451230638 ) ) ;
#9516 = B_SPLINE_CURVE_WITH_KNOTS ( 'NONE', 3,
 ( #1750, #7195, #10347, #919 ),
 .UNSPECIFIED., .F., .F.,
 ( 4, 4 ),
 ( 0.000000000000000000, 0.8724294488011775650 ),
 .UNSPECIFIED. ) ;
#9517 = ORIENTED_EDGE ( 'NONE', *, *, #13340, .T. ) ;
#9518 = DIRECTION ( 'NONE',  ( 0.000000000000000000, 1.000000000000000000, 0.000000000000000000 ) ) ;
#9519 = CIRCLE ( 'NONE', #5778, 14.25000000000000178 ) ;
#9520 = LINE ( 'NONE', #990, #2317 ) ;
#9521 = VECTOR ( 'NONE', #11135, 1000.000000000000000 ) ;
#9522 = CIRCLE ( 'NONE', #6872, 14.25000000000000178 ) ;
#9523 = CARTESIAN_POINT ( 'NONE',  ( -2.604399508763951321, 0.000000000000000000, 11.80615107470197422 ) ) ;
#9524 = DIRECTION ( 'NONE',  ( -0.000000000000000000, -1.000000000000000000, -0.000000000000000000 ) ) ;
#9525 = CARTESIAN_POINT ( 'NONE',  ( 12.01285915242476499, 3.000000000000000000, -4.000000001073668265 ) ) ;
#9526 = CARTESIAN_POINT ( 'NONE',  ( 12.00000000000000711, 5.000000000000000888, -10.00000000000000000 ) ) ;
#9527 = B_SPLINE_SURFACE_WITH_KNOTS ( 'NONE', 3, 1, ( 
 ( #12995, #7626 ),
 ( #9882, #5683 ),
 ( #533, #7757 ),
 ( #11065, #10990 ) ),
 .UNSPECIFIED., .F., .F., .F.,
 ( 4, 4 ),
 ( 2, 2 ),
 ( 0.000000000000000000, 0.8724294488011765658 ),
 ( 0.000000000000000000, 1.000000000000000000 ),
 .UNSPECIFIED. ) ;
#9528 = FACE_OUTER_BOUND ( 'NONE', #310, .T. ) ;
#9529 = CARTESIAN_POINT ( 'NONE',  ( -8.795158114916672432, 3.000000000000000000, -9.573149624528774382 ) ) ;
#9530 = ORIENTED_EDGE ( 'NONE', *, *, #8611, .T. ) ;
#9531 = CARTESIAN_POINT ( 'NONE',  ( 4.072642252455978884, 0.000000000000000000, 12.14623037080101042 ) ) ;
#9532 = ADVANCED_FACE ( 'NONE', ( #5791 ), #9015, .F. ) ;
#9533 = ORIENTED_EDGE ( 'NONE', *, *, #8038, .F. ) ;
#9534 = CIRCLE ( 'NONE', #4921, 12.00000000000000000 ) ;
#9535 = PRODUCT_DEFINITION_SHAPE ( 'NONE', 'NONE',  #13604 ) ;
#9536 = VERTEX_POINT ( 'NONE', #8068 ) ;
#9537 = CIRCLE ( 'NONE', #6892, 1.499999999686092877 ) ;
#9538 = CIRCLE ( 'NONE', #2259, 12.08999999999737440 ) ;
#9539 = ORIENTED_EDGE ( 'NONE', *, *, #2733, .T. ) ;
#9540 = EDGE_CURVE ( 'NONE', #11098, #12786, #488, .T. ) ;
#9541 = EDGE_CURVE ( 'NONE', #7012, #6815, #12733, .T. ) ;
#9542 = LINE ( 'NONE', #6507, #2281 ) ;
#9543 = DIRECTION ( 'NONE',  ( 0.000000000000000000, 0.000000000000000000, 1.000000000000000000 ) ) ;
#9544 = VECTOR ( 'NONE', #6246, 1000.000000000000000 ) ;
#9545 = DIRECTION ( 'NONE',  ( -0.000000000000000000, -1.000000000000000000, -0.000000000000000000 ) ) ;
#9546 = VECTOR ( 'NONE', #7441, 1000.000000000000000 ) ;
#9547 = DIRECTION ( 'NONE',  ( 0.000000000000000000, 0.000000000000000000, 1.000000000000000000 ) ) ;
#9548 = CARTESIAN_POINT ( 'NONE',  ( 7.712570079660896916, 0.000000000000000000, -11.14709020439929432 ) ) ;
#9549 = CARTESIAN_POINT ( 'NONE',  ( 8.914835885878220623, 3.000000000000000000, -11.11702303352196708 ) ) ;
#9550 = EDGE_CURVE ( 'NONE', #7235, #10564, #1556, .T. ) ;
#9551 = EDGE_LOOP ( 'NONE', ( #1149, #3802, #9530, #11820 ) ) ;
#9552 = VERTEX_POINT ( 'NONE', #4767 ) ;
#9553 = CARTESIAN_POINT ( 'NONE',  ( 30.73000000000000043, 3.000000000000000000, -3.999999999999999112 ) ) ;
#9554 = B_SPLINE_CURVE_WITH_KNOTS ( 'NONE', 3,
 ( #8817, #2631, #3728, #9928 ),
 .UNSPECIFIED., .F., .F.,
 ( 4, 4 ),
 ( 0.000000000000000000, 0.5855695330273008592 ),
 .UNSPECIFIED. ) ;
#9555 = VECTOR ( 'NONE', #603, 1000.000000000000000 ) ;
#9556 = AXIS2_PLACEMENT_3D ( 'NONE', #583, #5877, #1614 ) ;
#9557 = ORIENTED_EDGE ( 'NONE', *, *, #3064, .F. ) ;
#9558 = CARTESIAN_POINT ( 'NONE',  ( -12.40340517008309185, 0.000000000000000000, -3.893011711613028947 ) ) ;
#9559 = FACE_OUTER_BOUND ( 'NONE', #1484, .T. ) ;
#9560 = DIRECTION ( 'NONE',  ( 0.000000000000000000, 1.000000000000000000, -0.000000000000000000 ) ) ;
#9561 = CARTESIAN_POINT ( 'NONE',  ( 2.428572470324196431, 3.000000000000000000, 13.33579367773357127 ) ) ;
#9562 = AXIS2_PLACEMENT_3D ( 'NONE', #5001, #9195, #1914 ) ;
#9563 = DIRECTION ( 'NONE',  ( -0.000000000000000000, -1.000000000000000000, -0.000000000000000000 ) ) ;
#9564 = AXIS2_PLACEMENT_3D ( 'NONE', #10500, #2028, #6153 ) ;
#9565 = EDGE_CURVE ( 'NONE', #10765, #1237, #10398, .T. ) ;
#9566 = DIRECTION ( 'NONE',  ( 0.000000000000000000, 1.000000000000000000, -0.000000000000000000 ) ) ;
#9567 = AXIS2_PLACEMENT_3D ( 'NONE', #790, #7194, #10423 ) ;
#9568 = CARTESIAN_POINT ( 'NONE',  ( 52.12339130828321032, 0.000000000000000000, -4.353525159591052685 ) ) ;
#9569 = ORIENTED_EDGE ( 'NONE', *, *, #2793, .T. ) ;
#9570 = VERTEX_POINT ( 'NONE', #699 ) ;
#9571 = ORIENTED_EDGE ( 'NONE', *, *, #690, .F. ) ;
#9572 = EDGE_LOOP ( 'NONE', ( #477, #1005, #485, #9333 ) ) ;
#9573 = DIRECTION ( 'NONE',  ( 0.000000000000000000, 0.000000000000000000, 1.000000000000000000 ) ) ;
#9574 = SHAPE_REPRESENTATION_RELATIONSHIP ( 'NONE' , 'NONE' ,  #7939, #3921 ) ;
#9575 = CARTESIAN_POINT ( 'NONE',  ( 3.647470871583629926, 3.000000000000000000, -11.52666717836884125 ) ) ;
#9576 = DIRECTION ( 'NONE',  ( -0.000000000000000000, -1.000000000000000000, -0.000000000000000000 ) ) ;
#9577 = CARTESIAN_POINT ( 'NONE',  ( -7.668956737359326148, 9.000000000000000000, -2.066866683227997825 ) ) ;
#9578 = CARTESIAN_POINT ( 'NONE',  ( -4.564691384634503635, 3.000000000000000000, 12.76342233970727769 ) ) ;
#9579 = FACE_OUTER_BOUND ( 'NONE', #1308, .T. ) ;
#9580 = ORIENTED_EDGE ( 'NONE', *, *, #2950, .T. ) ;
#9581 = SURFACE_STYLE_FILL_AREA ( #9643 ) ;
#9582 = ORIENTED_EDGE ( 'NONE', *, *, #11631, .T. ) ;
#9583 = CIRCLE ( 'NONE', #10215, 14.24999999999999822 ) ;
#9584 = VERTEX_POINT ( 'NONE', #4694 ) ;
#9585 = ORIENTED_EDGE ( 'NONE', *, *, #5592, .F. ) ;
#9586 = DIRECTION ( 'NONE',  ( -0.000000000000000000, -1.000000000000000000, -0.000000000000000000 ) ) ;
#9587 = ORIENTED_EDGE ( 'NONE', *, *, #11489, .F. ) ;
#9588 = CARTESIAN_POINT ( 'NONE',  ( 20.00000000000000355, 3.000000000000000000, -14.92471123914604370 ) ) ;
#9589 = CARTESIAN_POINT ( 'NONE',  ( -3.542894779577211661, 3.000000000000000000, -12.51336118825813948 ) ) ;
#9590 = FACE_OUTER_BOUND ( 'NONE', #11303, .T. ) ;
#9591 = CARTESIAN_POINT ( 'NONE',  ( -13.49999999999999645, 3.000000000000000000, -7.049999999999998934 ) ) ;
#9592 = DIRECTION ( 'NONE',  ( 1.000000000000000000, -0.000000000000000000, 0.000000000000000000 ) ) ;
#9593 = EDGE_CURVE ( 'NONE', #180, #1668, #4448, .T. ) ;
#9594 = DIRECTION ( 'NONE',  ( 0.000000000000000000, 1.000000000000000000, 0.000000000000000000 ) ) ;
#9595 = FACE_OUTER_BOUND ( 'NONE', #767, .T. ) ;
#9596 = DIRECTION ( 'NONE',  ( 0.000000000000000000, 0.000000000000000000, 1.000000000000000000 ) ) ;
#9597 = CARTESIAN_POINT ( 'NONE',  ( -14.90895795148409420, 0.000000000000000000, 1.650143266773909101 ) ) ;
#9598 = ORIENTED_EDGE ( 'NONE', *, *, #8585, .T. ) ;
#9599 = DIRECTION ( 'NONE',  ( -0.000000000000000000, -1.000000000000000000, -0.000000000000000000 ) ) ;
#9600 = VERTEX_POINT ( 'NONE', #4893 ) ;
#9601 = ORIENTED_EDGE ( 'NONE', *, *, #1901, .T. ) ;
#9602 =( REPRESENTATION_RELATIONSHIP ('NONE','NONE', #3798, #8376 ) REPRESENTATION_RELATIONSHIP_WITH_TRANSFORMATION ( #3604 )SHAPE_REPRESENTATION_RELATIONSHIP( ) );
#9603 = ORIENTED_EDGE ( 'NONE', *, *, #1455, .T. ) ;
#9604 = CARTESIAN_POINT ( 'NONE',  ( 8.373678438139048552, 0.000000000000000000, 1.459968977288628844 ) ) ;
#9605 = CARTESIAN_POINT ( 'NONE',  ( 1.557181465540672161, 0.000000000000000000, -14.16466328168010591 ) ) ;
#9606 = EDGE_CURVE ( 'NONE', #6828, #12771, #8619, .T. ) ;
#9607 = ADVANCED_FACE ( 'NONE', ( #1738 ), #3787, .F. ) ;
#9608 = CARTESIAN_POINT ( 'NONE',  ( -6.549210654805285969, 9.000000000000000000, 1.634117437329680067 ) ) ;
#9609 = CARTESIAN_POINT ( 'NONE',  ( 8.504652361247167391, 3.000000000000000000, 9.593885948927674434 ) ) ;
#9610 = CARTESIAN_POINT ( 'NONE',  ( 0.000000000000000000, 3.000000000000000000, 0.000000000000000000 ) ) ;
#9611 = ADVANCED_FACE ( 'NONE', ( #570 ), #7851, .T. ) ;
#9612 = CARTESIAN_POINT ( 'NONE',  ( -5.250000000000000000, 3.000000000000000000, -27.94078293894052578 ) ) ;
#9613 = ADVANCED_FACE ( 'NONE', ( #7995 ), #276, .F. ) ;
#9614 = VERTEX_POINT ( 'NONE', #11167 ) ;
#9615 = EDGE_LOOP ( 'NONE', ( #11143, #8855, #2227, #9517 ) ) ;
#9616 = CARTESIAN_POINT ( 'NONE',  ( 8.430890348300625448, 3.000000000000000000, 11.48836750521723893 ) ) ;
#9617 = PRODUCT ( 'MAT-047', 'MAT-047', '', ( #6120 ) ) ;
#9618 = ORIENTED_EDGE ( 'NONE', *, *, #388, .F. ) ;
#9619 = CARTESIAN_POINT ( 'NONE',  ( 6.970598036433451661, 3.000000000000000000, -10.97318381393796294 ) ) ;
#9620 = CYLINDRICAL_SURFACE ( 'NONE', #5479, 14.25000000000000178 ) ;
#9621 = CARTESIAN_POINT ( 'NONE',  ( 26.30958424017656938, 0.1000000000000000056, 1.399999999999999911 ) ) ;
#9622 = CARTESIAN_POINT ( 'NONE',  ( 5.170206418547656391, 3.000000000000000000, 13.27898586450067064 ) ) ;
#9623 = CARTESIAN_POINT ( 'NONE',  ( -8.158551673544545579, 0.000000000000000000, 8.922226997226644585 ) ) ;
#9624 = EDGE_CURVE ( 'NONE', #12193, #12045, #4226, .T. ) ;
#9625 = LINE ( 'NONE', #2392, #11775 ) ;
#9626 = DIRECTION ( 'NONE',  ( 0.000000000000000000, 1.000000000000000000, 0.000000000000000000 ) ) ;
#9627 = ORIENTED_EDGE ( 'NONE', *, *, #8038, .T. ) ;
#9628 = ORIENTED_EDGE ( 'NONE', *, *, #13446, .T. ) ;
#9629 = ORIENTED_EDGE ( 'NONE', *, *, #1522, .F. ) ;
#9630 = CARTESIAN_POINT ( 'NONE',  ( -3.469446951953614189E-15, 2.000000000000000000, -6.999999999999998224 ) ) ;
#9631 = ORIENTED_EDGE ( 'NONE', *, *, #6943, .T. ) ;
#9632 = EDGE_CURVE ( 'NONE', #12628, #12207, #8937, .T. ) ;
#9633 = EDGE_CURVE ( 'NONE', #4532, #12628, #1385, .T. ) ;
#9634 = CYLINDRICAL_SURFACE ( 'NONE', #12972, 3.500000000000000888 ) ;
#9635 =( LENGTH_UNIT ( ) NAMED_UNIT ( * ) SI_UNIT ( .MILLI., .METRE. ) );
#9636 = CARTESIAN_POINT ( 'NONE',  ( 48.80418793193314997, 3.000000000000000000, -4.004112872419501201 ) ) ;
#9637 = FACE_OUTER_BOUND ( 'NONE', #12547, .T. ) ;
#9638 = PRODUCT_DEFINITION_SHAPE ( 'NONE', 'NONE',  #13607 ) ;
#9639 = DIRECTION ( 'NONE',  ( 0.000000000000000000, 0.000000000000000000, 1.000000000000000000 ) ) ;
#9640 = CARTESIAN_POINT ( 'NONE',  ( -3.647470871583628593, 3.000000000000000000, 11.52666717836884125 ) ) ;
#9641 = CARTESIAN_POINT ( 'NONE',  ( -13.17831234185052836, 0.000000000000000000, -4.227250083625696320 ) ) ;
#9642 = ORIENTED_EDGE ( 'NONE', *, *, #11133, .T. ) ;
#9643 = FILL_AREA_STYLE ('',( #95 ) ) ;
#9644 = ORIENTED_EDGE ( 'NONE', *, *, #11479, .F. ) ;
#9645 = ORIENTED_EDGE ( 'NONE', *, *, #3044, .F. ) ;
#9646 = ORIENTED_EDGE ( 'NONE', *, *, #11804, .F. ) ;
#9647 = DIRECTION ( 'NONE',  ( -0.000000000000000000, -1.000000000000000000, -0.000000000000000000 ) ) ;
#9648 = EDGE_LOOP ( 'NONE', ( #11112, #7980, #656, #3688 ) ) ;
#9649 = EDGE_CURVE ( 'NONE', #7142, #11145, #9430, .T. ) ;
#9650 = CARTESIAN_POINT ( 'NONE',  ( 1.650143266773734796, 3.000000000000000000, -14.90895795148410841 ) ) ;
#9651 = CYLINDRICAL_SURFACE ( 'NONE', #12462, 1.499999999999999556 ) ;
#9652 = CARTESIAN_POINT ( 'NONE',  ( -8.914835885878215294, 0.000000000000000000, 11.11702303352197063 ) ) ;
#9653 = FACE_OUTER_BOUND ( 'NONE', #10835, .T. ) ;
#9654 = CARTESIAN_POINT ( 'NONE',  ( 0.000000000000000000, 3.000000000000000000, 0.000000000000000000 ) ) ;
#9655 = B_SPLINE_CURVE_WITH_KNOTS ( 'NONE', 3,
 ( #11535, #7264, #929, #5124 ),
 .UNSPECIFIED., .F., .F.,
 ( 4, 4 ),
 ( 0.000000000000000000, 0.8724294488011786752 ),
 .UNSPECIFIED. ) ;
#9656 = CARTESIAN_POINT ( 'NONE',  ( 2.830255545554135832, 3.000000000000000000, -12.68816982652952596 ) ) ;
#9657 = DIRECTION ( 'NONE',  ( 0.000000000000000000, 1.000000000000000000, 0.000000000000000000 ) ) ;
#9658 = DIRECTION ( 'NONE',  ( 1.000000000000000000, 0.000000000000000000, -1.370446048119726253E-16 ) ) ;
#9659 = EDGE_LOOP ( 'NONE', ( #1523, #11667, #11698, #4140 ) ) ;
#9660 = CARTESIAN_POINT ( 'NONE',  ( 0.000000000000000000, 0.000000000000000000, 0.000000000000000000 ) ) ;
#9661 = ORIENTED_EDGE ( 'NONE', *, *, #2381, .T. ) ;
#9662 = VERTEX_POINT ( 'NONE', #420 ) ;
#9663 = ADVANCED_FACE ( 'NONE', ( #837 ), #5993, .T. ) ;
#9664 = ORIENTED_EDGE ( 'NONE', *, *, #8769, .T. ) ;
#9665 = AXIS2_PLACEMENT_3D ( 'NONE', #5416, #5154, #65 ) ;
#9666 = DIRECTION ( 'NONE',  ( -0.000000000000000000, -1.000000000000000000, -0.000000000000000000 ) ) ;
#9667 = CARTESIAN_POINT ( 'NONE',  ( -0.7702044561450404059, 0.000000000000000000, 12.79759916868914793 ) ) ;
#9668 = DIRECTION ( 'NONE',  ( 0.000000000000000000, 1.000000000000000000, 0.000000000000000000 ) ) ;
#9669 = CYLINDRICAL_SURFACE ( 'NONE', #6846, 2.750000000000002665 ) ;
#9670 = CARTESIAN_POINT ( 'NONE',  ( -12.08646469655240097, 0.000000000000000000, -8.883544964651921561 ) ) ;
#9671 = CARTESIAN_POINT ( 'NONE',  ( -5.999999999999991118, 3.000000000000000000, 28.50000000000000000 ) ) ;
#9672 = VECTOR ( 'NONE', #5066, 1000.000000000000000 ) ;
#9673 = CIRCLE ( 'NONE', #665, 3.499999999999999556 ) ;
#9674 = EDGE_LOOP ( 'NONE', ( #2112, #6293, #7632, #6618 ) ) ;
#9675 = VERTEX_POINT ( 'NONE', #10271 ) ;
#9676 = CARTESIAN_POINT ( 'NONE',  ( 4.355042381134428098, 0.000000000000000000, 7.299562031966232212 ) ) ;
#9677 = EDGE_CURVE ( 'NONE', #7207, #6405, #6978, .T. ) ;
#9678 = ORIENTED_EDGE ( 'NONE', *, *, #6010, .F. ) ;
#9679 = LINE ( 'NONE', #3214, #6678 ) ;
#9680 = CIRCLE ( 'NONE', #3741, 3.000000000000000444 ) ;
#9681 = VECTOR ( 'NONE', #838, 1000.000000000000000 ) ;
#9682 = CARTESIAN_POINT ( 'NONE',  ( -8.430890348300124515, 3.000000000000000000, 11.48836750521761019 ) ) ;
#9683 = FACE_BOUND ( 'NONE', #2141, .T. ) ;
#9684 = CARTESIAN_POINT ( 'NONE',  ( -12.08646469655240097, 3.000000000000000000, -8.883544964651921561 ) ) ;
#9685 = CARTESIAN_POINT ( 'NONE',  ( -13.97385902380755240, 3.000000000000000000, -5.452638258930474713 ) ) ;
#9686 = CARTESIAN_POINT ( 'NONE',  ( 5.250000000000000000, 0.000000000000000000, -26.44078293894052578 ) ) ;
#9687 = FACE_OUTER_BOUND ( 'NONE', #2889, .T. ) ;
#9688 = VERTEX_POINT ( 'NONE', #4069 ) ;
#9689 = VECTOR ( 'NONE', #13291, 1000.000000000000000 ) ;
#9690 = EDGE_CURVE ( 'NONE', #12613, #3990, #5340, .T. ) ;
#9691 = ORIENTED_EDGE ( 'NONE', *, *, #788, .T. ) ;
#9692 = CIRCLE ( 'NONE', #6619, 12.08999999999737440 ) ;
#9693 = VERTEX_POINT ( 'NONE', #6131 ) ;
#9694 = EDGE_LOOP ( 'NONE', ( #13280, #3951, #10363, #10088 ) ) ;
#9695 = CARTESIAN_POINT ( 'NONE',  ( -8.760376775873710997, 3.000000000000000000, 10.34346111134700941 ) ) ;
#9696 = ORIENTED_EDGE ( 'NONE', *, *, #212, .F. ) ;
#9697 = ADVANCED_FACE ( 'NONE', ( #5029 ), #11, .F. ) ;
#9698 = EDGE_CURVE ( 'NONE', #10414, #1535, #11898, .T. ) ;
#9699 = CYLINDRICAL_SURFACE ( 'NONE', #2623, 12.00000000000000000 ) ;
#9700 = AXIS2_PLACEMENT_3D ( 'NONE', #10308, #320, #8560 ) ;
#9701 = CARTESIAN_POINT ( 'NONE',  ( 6.000000000000008882, 3.000000000000000000, 27.00000000000000000 ) ) ;
#9702 = CARTESIAN_POINT ( 'NONE',  ( 0.000000000000000000, 3.000000000000000000, -1.500000000000000222 ) ) ;
#9703 = DIRECTION ( 'NONE',  ( 0.000000000000000000, 0.000000000000000000, 1.000000000000000000 ) ) ;
#9704 = DIRECTION ( 'NONE',  ( 0.000000000000000000, 0.000000000000000000, -1.000000000000000000 ) ) ;
#9705 = ORIENTED_EDGE ( 'NONE', *, *, #6794, .F. ) ;
#9706 = FACE_OUTER_BOUND ( 'NONE', #9615, .T. ) ;
#9707 = VERTEX_POINT ( 'NONE', #3092 ) ;
#9708 = ADVANCED_FACE ( 'NONE', ( #10205 ), #13574, .T. ) ;
#9709 = ORIENTED_EDGE ( 'NONE', *, *, #6232, .T. ) ;
#9710 = ORIENTED_EDGE ( 'NONE', *, *, #4648, .F. ) ;
#9711 = PLANE ( 'NONE',  #11274 ) ;
#9712 = VECTOR ( 'NONE', #8467, 1000.000000000000000 ) ;
#9713 = ORIENTED_EDGE ( 'NONE', *, *, #720, .F. ) ;
#9714 = EDGE_LOOP ( 'NONE', ( #7603, #4594, #747, #13056 ) ) ;
#9715 = DIRECTION ( 'NONE',  ( 0.000000000000000000, 1.000000000000000000, -0.000000000000000000 ) ) ;
#9716 = SURFACE_STYLE_FILL_AREA ( #2489 ) ;
#9717 = LINE ( 'NONE', #12832, #7320 ) ;
#9718 = LINE ( 'NONE', #3311, #4620 ) ;
#9719 = CARTESIAN_POINT ( 'NONE',  ( 2.604399508763947768, 3.000000000000000000, -11.80615107470197778 ) ) ;
#9720 = AXIS2_PLACEMENT_3D ( 'NONE', #6957, #8939, #12200 ) ;
#9721 = CARTESIAN_POINT ( 'NONE',  ( 55.44259468463320673, 0.000000000000000000, -4.702937446762657459 ) ) ;
#9722 = CARTESIAN_POINT ( 'NONE',  ( -3.835481108877868195, 1.734723475976807094E-15, 5.554420281491219136 ) ) ;
#9723 = ORIENTED_EDGE ( 'NONE', *, *, #13083, .T. ) ;
#9724 = CARTESIAN_POINT ( 'NONE',  ( 45.60964950616533287, 3.000000000000000000, -14.50984893380129392 ) ) ;
#9725 = B_SPLINE_SURFACE_WITH_KNOTS ( 'NONE', 3, 1, ( 
 ( #492, #11169 ),
 ( #4695, #6896 ),
 ( #8887, #3033 ),
 ( #10408, #11510 ) ),
 .UNSPECIFIED., .F., .F., .F.,
 ( 4, 4 ),
 ( 2, 2 ),
 ( 0.5454515525569062495, 0.5748696296145745510 ),
 ( 0.000000000000000000, 1.000000000000000000 ),
 .UNSPECIFIED. ) ;
#9726 = EDGE_CURVE ( 'NONE', #12940, #12096, #10850, .T. ) ;
#9727 = ORIENTED_EDGE ( 'NONE', *, *, #6200, .F. ) ;
#9728 = EDGE_LOOP ( 'NONE', ( #2294, #6729, #10216, #2371 ) ) ;
#9729 = ORIENTED_EDGE ( 'NONE', *, *, #12851, .F. ) ;
#9730 = VECTOR ( 'NONE', #7987, 1000.000000000000000 ) ;
#9731 = AXIS2_PLACEMENT_3D ( 'NONE', #11859, #104, #8480 ) ;
#9732 = VECTOR ( 'NONE', #11190, 1000.000000000000000 ) ;
#9733 = CARTESIAN_POINT ( 'NONE',  ( -14.39763212228012534, 3.000000000000000000, 1.133238802859812155 ) ) ;
#9734 = CYLINDRICAL_SURFACE ( 'NONE', #1209, 0.1000000000000000472 ) ;
#9735 = DIRECTION ( 'NONE',  ( -0.6291930273682743158, 0.000000000000000000, 0.7772490812546168915 ) ) ;
#9736 = DIRECTION ( 'NONE',  ( -0.000000000000000000, -0.000000000000000000, -1.000000000000000000 ) ) ;
#9737 = CARTESIAN_POINT ( 'NONE',  ( -12.68816982652953840, 0.000000000000000000, -2.830255545554093644 ) ) ;
#9738 = AXIS2_PLACEMENT_3D ( 'NONE', #3690, #13205, #12113 ) ;
#9739 = DIRECTION ( 'NONE',  ( -0.000000000000000000, -1.000000000000000000, -0.000000000000000000 ) ) ;
#9740 = VECTOR ( 'NONE', #4104, 1000.000000000000114 ) ;
#9741 = VECTOR ( 'NONE', #9777, 1000.000000000000000 ) ;
#9742 = ORIENTED_EDGE ( 'NONE', *, *, #7339, .F. ) ;
#9743 = EDGE_LOOP ( 'NONE', ( #8956, #1499, #5724, #12403, #5324, #5425 ) ) ;
#9744 = CARTESIAN_POINT ( 'NONE',  ( 31.00000000000000000, 2.900000000000000355, -1.600000000000004086 ) ) ;
#9745 = ORIENTED_EDGE ( 'NONE', *, *, #4799, .T. ) ;
#9746 = FACE_OUTER_BOUND ( 'NONE', #3486, .T. ) ;
#9747 = AXIS2_PLACEMENT_3D ( 'NONE', #3818, #10083, #3946 ) ;
#9748 = PRODUCT_DEFINITION_SHAPE ( 'NONE', 'NONE',  #13617 ) ;
#9749 = TOROIDAL_SURFACE ( 'NONE', #7342, 3.100000000000000533, 0.1000000000000000056 ) ;
#9750 = AXIS2_PLACEMENT_3D ( 'NONE', #2735, #7826, #12044 ) ;
#9751 = CARTESIAN_POINT ( 'NONE',  ( -2.375523406013128724, 9.000000000000000000, 6.318179211409233886 ) ) ;
#9752 = DIRECTION ( 'NONE',  ( 0.000000000000000000, 0.000000000000000000, 1.000000000000000000 ) ) ;
#9753 = CARTESIAN_POINT ( 'NONE',  ( -7.500000000000000000, 3.000000000000000000, 1.500000000000000666 ) ) ;
#9754 = CARTESIAN_POINT ( 'NONE',  ( 6.000000000000008882, 3.000000000000000000, 28.50000000000000000 ) ) ;
#9755 = ADVANCED_FACE ( 'NONE', ( #1939 ), #1486, .F. ) ;
#9756 = LINE ( 'NONE', #11692, #9119 ) ;
#9757 = CARTESIAN_POINT ( 'NONE',  ( -7.500000000000000000, 3.000000000000000000, 0.000000000000000000 ) ) ;
#9758 = CARTESIAN_POINT ( 'NONE',  ( 4.577511697546072789, 0.000000000000000000, 12.75843939030335505 ) ) ;
#9759 = AXIS2_PLACEMENT_3D ( 'NONE', #13, #12358, #8196 ) ;
#9760 = ORIENTED_EDGE ( 'NONE', *, *, #6082, .F. ) ;
#9761 = ORIENTED_EDGE ( 'NONE', *, *, #7406, .F. ) ;
#9762 = VERTEX_POINT ( 'NONE', #3924 ) ;
#9763 = VERTEX_POINT ( 'NONE', #10331 ) ;
#9764 = CARTESIAN_POINT ( 'NONE',  ( 31.00000000000000000, 3.000000000000000000, 1.499999998612421725 ) ) ;
#9765 = ORIENTED_EDGE ( 'NONE', *, *, #4376, .T. ) ;
#9766 = DIRECTION ( 'NONE',  ( -0.000000000000000000, -1.000000000000000000, -0.000000000000000000 ) ) ;
#9767 = AXIS2_PLACEMENT_3D ( 'NONE', #11060, #7683, #5892 ) ;
#9768 = CIRCLE ( 'NONE', #13526, 0.9999999999999997780 ) ;
#9769 = EDGE_CURVE ( 'NONE', #7333, #4390, #12493, .T. ) ;
#9770 = DIRECTION ( 'NONE',  ( -0.000000000000000000, -1.000000000000000000, -0.000000000000000000 ) ) ;
#9771 = AXIS2_PLACEMENT_3D ( 'NONE', #7051, #4490, #6488 ) ;
#9772 = CARTESIAN_POINT ( 'NONE',  ( 0.000000000000000000, 0.000000000000000000, 0.000000000000000000 ) ) ;
#9773 = CARTESIAN_POINT ( 'NONE',  ( -4.499999999999993783, 0.000000000000000000, 13.39999999999999858 ) ) ;
#9774 = CARTESIAN_POINT ( 'NONE',  ( 0.000000000000000000, 9.000000000000000000, 0.000000000000000000 ) ) ;
#9775 = ORIENTED_EDGE ( 'NONE', *, *, #10040, .F. ) ;
#9776 = EDGE_CURVE ( 'NONE', #1742, #45, #12405, .T. ) ;
#9777 = DIRECTION ( 'NONE',  ( -0.000000000000000000, -1.000000000000000000, -0.000000000000000000 ) ) ;
#9778 = EDGE_LOOP ( 'NONE', ( #6008, #5649, #6887, #7891 ) ) ;
#9779 = EDGE_CURVE ( 'NONE', #9763, #1814, #10581, .T. ) ;
#9780 = ORIENTED_EDGE ( 'NONE', *, *, #3438, .T. ) ;
#9781 = VERTEX_POINT ( 'NONE', #4131 ) ;
#9782 = CIRCLE ( 'NONE', #7586, 3.000000000000000888 ) ;
#9783 = CARTESIAN_POINT ( 'NONE',  ( -2.411622991978541464, 9.000000000000000000, -6.304488444319688689 ) ) ;
#9784 = ORIENTED_EDGE ( 'NONE', *, *, #10547, .T. ) ;
#9785 = ORIENTED_EDGE ( 'NONE', *, *, #4789, .T. ) ;
#9786 = FACE_OUTER_BOUND ( 'NONE', #13221, .T. ) ;
#9787 = CARTESIAN_POINT ( 'NONE',  ( -3.647470871583628593, 3.000000000000000000, 11.52666717836884125 ) ) ;
#9788 = EDGE_CURVE ( 'NONE', #1110, #6430, #6229, .T. ) ;
#9789 = CARTESIAN_POINT ( 'NONE',  ( 9.133371500908369356, 0.000000000000000000, -11.90284147956862171 ) ) ;
#9790 = STYLED_ITEM ( 'NONE', ( #11100 ), #639 ) ;
#9791 = CARTESIAN_POINT ( 'NONE',  ( 4.690415759823430619, 2.900000000000000355, 4.500000000000000888 ) ) ;
#9792 = CIRCLE ( 'NONE', #8035, 1.499999999999997780 ) ;
#9793 = CARTESIAN_POINT ( 'NONE',  ( -0.8148820470561124463, 9.000000000000000000, 6.700631854488474204 ) ) ;
#9794 = B_SPLINE_CURVE_WITH_KNOTS ( 'NONE', 3,
 ( #13356, #2049, #12326, #12473 ),
 .UNSPECIFIED., .F., .F.,
 ( 4, 4 ),
 ( 0.000000000000000000, 0.8724294488011786752 ),
 .UNSPECIFIED. ) ;
#9795 = DIRECTION ( 'NONE',  ( 0.000000000000000000, 1.000000000000000000, -0.000000000000000000 ) ) ;
#9796 = EDGE_LOOP ( 'NONE', ( #11174, #3213, #2644, #2570 ) ) ;
#9797 = CARTESIAN_POINT ( 'NONE',  ( 5.958322434183389582, 0.000000000000000000, -6.062045345451230638 ) ) ;
#9798 = EDGE_CURVE ( 'NONE', #13005, #8655, #9303, .T. ) ;
#9799 = EDGE_LOOP ( 'NONE', ( #209, #9742, #6614, #6853 ) ) ;
#9800 = ORIENTED_EDGE ( 'NONE', *, *, #7671, .T. ) ;
#9801 = B_SPLINE_SURFACE_WITH_KNOTS ( 'NONE', 3, 1, ( 
 ( #12298, #13390 ),
 ( #5942, #714 ),
 ( #2840, #9320 ),
 ( #8141, #4913 ) ),
 .UNSPECIFIED., .F., .F., .F.,
 ( 4, 4 ),
 ( 2, 2 ),
 ( 0.000000000000000000, 0.8452273900860258760 ),
 ( 0.000000000000000000, 1.000000000000000000 ),
 .UNSPECIFIED. ) ;
#9802 = ORIENTED_EDGE ( 'NONE', *, *, #9565, .T. ) ;
#9803 = AXIS2_PLACEMENT_3D ( 'NONE', #7974, #2876, #549 ) ;
#9804 = DIRECTION ( 'NONE',  ( 0.000000000000000000, 1.000000000000000000, -0.000000000000000000 ) ) ;
#9805 = DIRECTION ( 'NONE',  ( 1.000000000000000000, -0.000000000000000000, -9.145772869372436484E-17 ) ) ;
#9806 = ADVANCED_FACE ( 'NONE', ( #5751 ), #8841, .T. ) ;
#9807 = ITEM_DEFINED_TRANSFORMATION ( 'NONE', 'NONE', #7181,  #10007 ) ;
#9808 = CARTESIAN_POINT ( 'NONE',  ( 7.940744365623959133, 9.000000000000000000, 0.1715058177969961128 ) ) ;
#9809 = FACE_OUTER_BOUND ( 'NONE', #7405, .T. ) ;
#9810 = DIRECTION ( 'NONE',  ( 0.000000000000000000, 0.000000000000000000, 1.000000000000000000 ) ) ;
#9811 = CARTESIAN_POINT ( 'NONE',  ( -2.604399508763951321, 3.000000000000000000, 11.80615107470197422 ) ) ;
#9812 = EDGE_CURVE ( 'NONE', #2852, #4189, #9254, .T. ) ;
#9813 = EDGE_LOOP ( 'NONE', ( #2515, #77 ) ) ;
#9814 = EDGE_LOOP ( 'NONE', ( #524, #9335, #637, #2070 ) ) ;
#9815 = DIRECTION ( 'NONE',  ( -0.000000000000000000, -1.000000000000000000, -0.000000000000000000 ) ) ;
#9816 = ORIENTED_EDGE ( 'NONE', *, *, #12822, .F. ) ;
#9817 = DIRECTION ( 'NONE',  ( 3.061616997868383141E-16, 0.000000000000000000, 1.000000000000000000 ) ) ;
#9818 = CARTESIAN_POINT ( 'NONE',  ( -6.343077614891082128, 0.000000000000000000, -11.35348748332310720 ) ) ;
#9819 = DIRECTION ( 'NONE',  ( 0.000000000000000000, 1.000000000000000000, -0.000000000000000000 ) ) ;
#9820 = CARTESIAN_POINT ( 'NONE',  ( 1.127406311874972422, 0.000000000000000000, -7.862174656777307646 ) ) ;
#9821 = CARTESIAN_POINT ( 'NONE',  ( 31.00000000000000000, 0.000000000000000000, -1.073670993220974656E-09 ) ) ;
#9822 = CARTESIAN_POINT ( 'NONE',  ( -12.08646469655240097, 0.000000000000000000, -8.883544964651921561 ) ) ;
#9823 = CARTESIAN_POINT ( 'NONE',  ( 2.719999999999997087, 0.000000000000000000, -7.500000000000000000 ) ) ;
#9824 = VERTEX_POINT ( 'NONE', #7753 ) ;
#9825 = ORIENTED_EDGE ( 'NONE', *, *, #7182, .T. ) ;
#9826 = EDGE_LOOP ( 'NONE', ( #6902, #2032, #2597, #4665, #3323, #1327, #8044, #7518, #4754, #6362, #9354, #2824, #11156, #1261, #1588, #8538, #1574, #6139, #4614, #324, #1912, #8810, #1663, #2723, #11754, #2926, #8597, #9192, #4361, #13004, #11205, #2996, #4569, #6066, #9126, #2188, #12582, #1557, #5873, #5872, #12558, #8725, #4759, #4223, #3300, #13373, #4346, #12894, #6241, #11089, #4578, #5629, #2166, #3421, #2539, #4483, #1745, #9533, #8550, #4478, #6717, #7447, #7385, #9489, #10871, #1775, #12505, #12579, #7566, #10967, #2238, #5760, #12340, #10689, #3920, #6703, #849, #8153, #7619, #9571, #8170, #6825, #13569, #5577, #831, #9678, #6564, #11977, #4802, #6034, #3459 ) ) ;
#9827 = ORIENTED_EDGE ( 'NONE', *, *, #4912, .F. ) ;
#9828 = CARTESIAN_POINT ( 'NONE',  ( -8.158551673544545579, 3.000000000000000000, 8.922226997226644585 ) ) ;
#9829 = ADVANCED_FACE ( 'NONE', ( #5682 ), #6670, .T. ) ;
#9830 = ORIENTED_EDGE ( 'NONE', *, *, #4743, .F. ) ;
#9831 = LINE ( 'NONE', #2469, #11650 ) ;
#9832 = SHAPE_REPRESENTATION_RELATIONSHIP ( 'NONE' , 'NONE' ,  #5135, #2434 ) ;
#9833 = B_SPLINE_SURFACE_WITH_KNOTS ( 'NONE', 3, 1, ( 
 ( #2125, #3913 ),
 ( #4120, #8117 ),
 ( #7093, #5284 ),
 ( #10322, #1027 ) ),
 .UNSPECIFIED., .F., .F., .F.,
 ( 4, 4 ),
 ( 2, 2 ),
 ( 0.2727224849193458089, 0.3021405619770169415 ),
 ( 0.000000000000000000, 1.000000000000000000 ),
 .UNSPECIFIED. ) ;
#9834 = CARTESIAN_POINT ( 'NONE',  ( -8.922226997226788470, 0.000000000000000000, -8.158551673544387484 ) ) ;
#9835 = CARTESIAN_POINT ( 'NONE',  ( 0.000000000000000000, 3.000000000000000000, 0.000000000000000000 ) ) ;
#9836 = CARTESIAN_POINT ( 'NONE',  ( 8.482622935103764306, 0.000000000000000000, -9.600126836553261711 ) ) ;
#9837 = CARTESIAN_POINT ( 'NONE',  ( -10.25006213149496936, 0.000000000000000000, -9.299128225235415712 ) ) ;
#9838 = VERTEX_POINT ( 'NONE', #6583 ) ;
#9839 = CYLINDRICAL_SURFACE ( 'NONE', #12620, 14.25000000000000000 ) ;
#9840 = VERTEX_POINT ( 'NONE', #9952 ) ;
#9841 = ORIENTED_EDGE ( 'NONE', *, *, #5889, .T. ) ;
#9842 = DIRECTION ( 'NONE',  ( 0.000000000000000000, 1.000000000000000000, 0.000000000000000000 ) ) ;
#9843 = ADVANCED_FACE ( 'NONE', ( #3619 ), #10537, .F. ) ;
#9844 = EDGE_CURVE ( 'NONE', #8260, #5689, #11967, .T. ) ;
#9845 = EDGE_LOOP ( 'NONE', ( #8721, #1944, #10981, #2966 ) ) ;
#9846 = EDGE_LOOP ( 'NONE', ( #11999, #100, #11073, #6032 ) ) ;
#9847 = DIRECTION ( 'NONE',  ( -0.000000000000000000, -1.000000000000000000, -0.000000000000000000 ) ) ;
#9848 = SURFACE_STYLE_USAGE ( .BOTH. , #12830 ) ;
#9849 = EDGE_CURVE ( 'NONE', #2082, #1008, #7754, .T. ) ;
#9850 = APPLICATION_CONTEXT ( 'automotive_design' ) ;
#9851 = CARTESIAN_POINT ( 'NONE',  ( -14.90895795148411374, 0.000000000000000000, -1.650143266773683726 ) ) ;
#9852 = CYLINDRICAL_SURFACE ( 'NONE', #1997, 1.499999999686092877 ) ;
#9853 = CARTESIAN_POINT ( 'NONE',  ( 2.161962830978694683, 0.000000000000000000, -14.08504230442587790 ) ) ;
#9854 = CARTESIAN_POINT ( 'NONE',  ( -13.52637830886122572, 3.000000000000000000, -2.928250210355275218 ) ) ;
#9855 = CARTESIAN_POINT ( 'NONE',  ( -12.98835496148299207, 0.000000000000000000, 0.5501230721524459355 ) ) ;
#9856 = ORIENTED_EDGE ( 'NONE', *, *, #4789, .F. ) ;
#9857 = VECTOR ( 'NONE', #9224, 1000.000000000000000 ) ;
#9858 = DIRECTION ( 'NONE',  ( 0.000000000000000000, 1.000000000000000000, 0.000000000000000000 ) ) ;
#9859 = ORIENTED_EDGE ( 'NONE', *, *, #6920, .T. ) ;
#9860 = ORIENTED_EDGE ( 'NONE', *, *, #10209, .F. ) ;
#9861 = EDGE_CURVE ( 'NONE', #8751, #5374, #3479, .T. ) ;
#9862 = ORIENTED_EDGE ( 'NONE', *, *, #11034, .T. ) ;
#9863 = CARTESIAN_POINT ( 'NONE',  ( 12.90250726680438476, 3.000000000000000000, 4.728042766759046778 ) ) ;
#9864 = ADVANCED_FACE ( 'NONE', ( #6722 ), #6654, .T. ) ;
#9865 = DIRECTION ( 'NONE',  ( 0.000000000000000000, 1.000000000000000000, -0.000000000000000000 ) ) ;
#9866 = ADVANCED_FACE ( 'NONE', ( #10861 ), #8728, .F. ) ;
#9867 = CARTESIAN_POINT ( 'NONE',  ( -0.6724118135763151871, 3.000000000000000000, -13.82336506795071784 ) ) ;
#9868 = CARTESIAN_POINT ( 'NONE',  ( 10.69794375946289655, 3.000000000000000000, 7.065816209474157006 ) ) ;
#9869 = DIRECTION ( 'NONE',  ( 0.000000000000000000, 0.000000000000000000, 1.000000000000000000 ) ) ;
#9870 = CARTESIAN_POINT ( 'NONE',  ( 13.50000000000000355, 3.000000000000000000, -7.050000000000000711 ) ) ;
#9871 = B_SPLINE_CURVE_WITH_KNOTS ( 'NONE', 3,
 ( #1976, #1013, #9343, #1073 ),
 .UNSPECIFIED., .F., .F.,
 ( 4, 4 ),
 ( 0.000000000000000000, 0.8452273900860258760 ),
 .UNSPECIFIED. ) ;
#9872 = CARTESIAN_POINT ( 'NONE',  ( -12.79759916868914615, 0.000000000000000000, -0.7702044561450367421 ) ) ;
#9873 = VERTEX_POINT ( 'NONE', #2136 ) ;
#9874 = VERTEX_POINT ( 'NONE', #6332 ) ;
#9875 = AXIS2_PLACEMENT_3D ( 'NONE', #7376, #2542, #3692 ) ;
#9876 = EDGE_CURVE ( 'NONE', #9536, #12679, #7766, .T. ) ;
#9877 = ORIENTED_EDGE ( 'NONE', *, *, #10073, .F. ) ;
#9878 = DIRECTION ( 'NONE',  ( -0.000000000000000000, -1.000000000000000000, -0.000000000000000000 ) ) ;
#9879 = DIRECTION ( 'NONE',  ( 0.000000000000000000, 0.000000000000000000, 1.000000000000000000 ) ) ;
#9880 = B_SPLINE_CURVE_WITH_KNOTS ( 'NONE', 3,
 ( #1123, #2992, #6221, #6094 ),
 .UNSPECIFIED., .F., .F.,
 ( 4, 4 ),
 ( 0.000000000000000000, 0.8724294488011765658 ),
 .UNSPECIFIED. ) ;
#9881 = DIRECTION ( 'NONE',  ( 0.000000000000000000, 0.000000000000000000, 1.000000000000000000 ) ) ;
#9882 = CARTESIAN_POINT ( 'NONE',  ( 4.164551629694410728, 9.000000000000000000, -6.072874324029720050 ) ) ;
#9883 = DIRECTION ( 'NONE',  ( 0.7216024245882217691, 0.000000000000000000, 0.6923076923076904032 ) ) ;
#9884 = CARTESIAN_POINT ( 'NONE',  ( -6.970598036433426792, 3.000000000000000000, -10.97318381393771780 ) ) ;
#9885 = CARTESIAN_POINT ( 'NONE',  ( -12.98835496148321944, 0.000000000000000000, -0.5501230721522551992 ) ) ;
#9886 = DIRECTION ( 'NONE',  ( 0.000000000000000000, 0.000000000000000000, 1.000000000000000000 ) ) ;
#9887 = ORIENTED_EDGE ( 'NONE', *, *, #12721, .T. ) ;
#9888 = EDGE_CURVE ( 'NONE', #1838, #2349, #4237, .T. ) ;
#9889 = ORIENTED_EDGE ( 'NONE', *, *, #6526, .F. ) ;
#9890 = ADVANCED_FACE ( 'NONE', ( #331 ), #7684, .T. ) ;
#9891 = VERTEX_POINT ( 'NONE', #5547 ) ;
#9892 = ORIENTED_EDGE ( 'NONE', *, *, #8860, .T. ) ;
#9893 = CARTESIAN_POINT ( 'NONE',  ( -0.1834773636644435324, 3.000000000000000000, -13.00394737445024873 ) ) ;
#9894 = VECTOR ( 'NONE', #6987, 1000.000000000000114 ) ;
#9895 = AXIS2_PLACEMENT_3D ( 'NONE', #7502, #1038, #9433 ) ;
#9896 = VERTEX_POINT ( 'NONE', #1428 ) ;
#9897 = DIRECTION ( 'NONE',  ( 0.000000000000000000, 1.000000000000000000, 0.000000000000000000 ) ) ;
#9898 =( LENGTH_UNIT ( ) NAMED_UNIT ( * ) SI_UNIT ( .MILLI., .METRE. ) );
#9899 = DIRECTION ( 'NONE',  ( 0.000000000000000000, 0.000000000000000000, 1.000000000000000000 ) ) ;
#9900 = CARTESIAN_POINT ( 'NONE',  ( 31.00000000000000000, 0.09999999999999982514, 0.000000000000000000 ) ) ;
#9901 = CARTESIAN_POINT ( 'NONE',  ( 0.000000000000000000, 0.09999999999999982514, 1.500000000000000000 ) ) ;
#9902 = CIRCLE ( 'NONE', #3305, 14.25000000000000178 ) ;
#9903 = DIRECTION ( 'NONE',  ( 0.000000000000000000, 0.000000000000000000, -1.000000000000000000 ) ) ;
#9904 = CIRCLE ( 'NONE', #12576, 1.000000000000000888 ) ;
#9905 = DIRECTION ( 'NONE',  ( -0.000000000000000000, -1.000000000000000000, -0.000000000000000000 ) ) ;
#9906 = ORIENTED_EDGE ( 'NONE', *, *, #3167, .T. ) ;
#9907 = FILL_AREA_STYLE_COLOUR ( '', #8197 ) ;
#9908 = VERTEX_POINT ( 'NONE', #5621 ) ;
#9909 = ORIENTED_EDGE ( 'NONE', *, *, #8755, .T. ) ;
#9910 = DIRECTION ( 'NONE',  ( 0.000000000000000000, -1.000000000000000000, -2.891205793294684736E-16 ) ) ;
#9911 = ORIENTED_EDGE ( 'NONE', *, *, #44, .T. ) ;
#9912 = CIRCLE ( 'NONE', #12790, 14.25000000000000178 ) ;
#9913 = ORIENTED_EDGE ( 'NONE', *, *, #5607, .F. ) ;
#9914 = CIRCLE ( 'NONE', #5523, 14.25000000000000000 ) ;
#9915 = CARTESIAN_POINT ( 'NONE',  ( -12.98835496148321944, 0.000000000000000000, -0.5501230721522550882 ) ) ;
#9916 = DIRECTION ( 'NONE',  ( -0.000000000000000000, -1.000000000000000000, -0.000000000000000000 ) ) ;
#9917 = FILL_AREA_STYLE ('',( #4768 ) ) ;
#9918 = CARTESIAN_POINT ( 'NONE',  ( 0.000000000000000000, 0.000000000000000000, 0.000000000000000000 ) ) ;
#9919 = CARTESIAN_POINT ( 'NONE',  ( 1.734723475976807094E-15, 0.000000000000000000, 7.000000000000000000 ) ) ;
#9920 = CARTESIAN_POINT ( 'NONE',  ( -0.7901945867173586491, 3.000000000000000000, -12.78643498603818074 ) ) ;
#9921 = EDGE_CURVE ( 'NONE', #6069, #10765, #9197, .T. ) ;
#9922 = VERTEX_POINT ( 'NONE', #8031 ) ;
#9923 = CARTESIAN_POINT ( 'NONE',  ( 5.170206418547656391, 3.000000000000000000, 13.27898586450067064 ) ) ;
#9924 = AXIS2_PLACEMENT_3D ( 'NONE', #779, #8269, #907 ) ;
#9925 = VERTEX_POINT ( 'NONE', #13194 ) ;
#9926 = ORIENTED_EDGE ( 'NONE', *, *, #10284, .F. ) ;
#9927 = VERTEX_POINT ( 'NONE', #1704 ) ;
#9928 = CARTESIAN_POINT ( 'NONE',  ( -12.98835496148321944, 3.000000000000000000, -0.5501230721522551992 ) ) ;
#9929 = DIRECTION ( 'NONE',  ( 1.000000000000000000, 0.000000000000000000, 0.000000000000000000 ) ) ;
#9930 = CIRCLE ( 'NONE', #7087, 8.499999999999992895 ) ;
#9931 = CARTESIAN_POINT ( 'NONE',  ( -13.33579367773357482, 3.000000000000000000, 2.428572470324200427 ) ) ;
#9932 = CARTESIAN_POINT ( 'NONE',  ( 7.499999999999999112, 3.000000000000000000, 1.499999999999997780 ) ) ;
#9933 = CARTESIAN_POINT ( 'NONE',  ( 0.8327827707325454742, 9.000000000000000000, 6.698430626405788679 ) ) ;
#9934 = B_SPLINE_SURFACE_WITH_KNOTS ( 'NONE', 2, 1, ( 
 ( #2993, #7442 ),
 ( #12690, #10611 ),
 ( #9326, #4343 ) ),
 .UNSPECIFIED., .F., .F., .F.,
 ( 3, 3 ),
 ( 2, 2 ),
 ( 0.000000000000000000, 1.000000000000000000 ),
 ( 0.000000000000000000, 1.000000000000000000 ),
 .UNSPECIFIED. ) ;
#9935 = EDGE_CURVE ( 'NONE', #578, #2082, #5962, .T. ) ;
#9936 = DIRECTION ( 'NONE',  ( -0.000000000000000000, 1.000000000000000000, -0.000000000000000000 ) ) ;
#9937 = CARTESIAN_POINT ( 'NONE',  ( -12.07793442604884682, 0.000000000000000000, 0.5400000000005513723 ) ) ;
#9938 = ADVANCED_FACE ( 'NONE', ( #1637 ), #8098, .F. ) ;
#9939 = CARTESIAN_POINT ( 'NONE',  ( -5.170206418547658167, 3.000000000000000000, -13.27898586450066887 ) ) ;
#9940 = ORIENTED_EDGE ( 'NONE', *, *, #2697, .T. ) ;
#9941 = CIRCLE ( 'NONE', #6002, 1.000000000000000000 ) ;
#9942 = EDGE_CURVE ( 'NONE', #6484, #5272, #811, .T. ) ;
#9943 = ORIENTED_EDGE ( 'NONE', *, *, #3970, .T. ) ;
#9944 = AXIS2_PLACEMENT_3D ( 'NONE', #6091, #8340, #10287 ) ;
#9945 = ADVANCED_FACE ( 'NONE', ( #10305 ), #2727, .T. ) ;
#9946 = CIRCLE ( 'NONE', #2479, 6.750000000000000888 ) ;
#9947 = B_SPLINE_SURFACE_WITH_KNOTS ( 'NONE', 3, 1, ( 
 ( #7805, #5734 ),
 ( #9931, #509 ),
 ( #1955, #796 ),
 ( #6145, #9243 ) ),
 .UNSPECIFIED., .F., .F., .F.,
 ( 4, 4 ),
 ( 2, 2 ),
 ( 0.000000000000000000, 0.8452273900860258760 ),
 ( 0.000000000000000000, 1.000000000000000000 ),
 .UNSPECIFIED. ) ;
#9948 = ORIENTED_EDGE ( 'NONE', *, *, #7589, .F. ) ;
#9949 = CARTESIAN_POINT ( 'NONE',  ( 5.797378255456016483, 3.000000000000000000, 12.25282671965375592 ) ) ;
#9950 = CARTESIAN_POINT ( 'NONE',  ( 6.749972395921142621, 9.000000000000000000, -0.01930425607464712062 ) ) ;
#9951 = AXIS2_PLACEMENT_3D ( 'NONE', #9294, #4125, #13507 ) ;
#9952 = CARTESIAN_POINT ( 'NONE',  ( 11.11702303352194043, 3.000000000000000000, -8.914835885878249044 ) ) ;
#9953 = AXIS2_PLACEMENT_3D ( 'NONE', #12102, #2653, #4858 ) ;
#9954 = VECTOR ( 'NONE', #5575, 1000.000000000000000 ) ;
#9955 = ADVANCED_FACE ( 'NONE', ( #2859 ), #13036, .F. ) ;
#9956 = DIRECTION ( 'NONE',  ( 0.000000000000000000, 0.000000000000000000, -1.000000000000000000 ) ) ;
#9957 = DIRECTION ( 'NONE',  ( -0.000000000000000000, -1.000000000000000000, -0.000000000000000000 ) ) ;
#9958 = CARTESIAN_POINT ( 'NONE',  ( 12.89546620003432764, 3.000000000000000000, -4.733530556166651415 ) ) ;
#9959 = DIRECTION ( 'NONE',  ( 0.000000000000000000, 0.000000000000000000, 1.000000000000000000 ) ) ;
#9960 = DIRECTION ( 'NONE',  ( 0.000000000000000000, 1.000000000000000000, 0.000000000000000000 ) ) ;
#9961 = ORIENTED_EDGE ( 'NONE', *, *, #3887, .T. ) ;
#9962 = ADVANCED_FACE ( 'NONE', ( #11062 ), #3141, .T. ) ;
#9963 = VERTEX_POINT ( 'NONE', #12390 ) ;
#9964 = VERTEX_POINT ( 'NONE', #10161 ) ;
#9965 = CIRCLE ( 'NONE', #11963, 1.500000000000000666 ) ;
#9966 = CARTESIAN_POINT ( 'NONE',  ( 11.70905276178455878, 0.000000000000000000, -9.375397774054460953 ) ) ;
#9967 = AXIS2_PLACEMENT_3D ( 'NONE', #8015, #12235, #2782 ) ;
#9968 = CIRCLE ( 'NONE', #3155, 14.25000000000000000 ) ;
#9969 = ORIENTED_EDGE ( 'NONE', *, *, #3182, .F. ) ;
#9970 = CARTESIAN_POINT ( 'NONE',  ( 0.000000000000000000, 13.00000000000000178, -1.500000000000000222 ) ) ;
#9971 = DIRECTION ( 'NONE',  ( 0.7679577490033002718, 0.000000000000000000, 0.6405005040948713591 ) ) ;
#9972 = LINE ( 'NONE', #3494, #7286 ) ;
#9973 = CARTESIAN_POINT ( 'NONE',  ( 2.999999999999995559, 0.000000000000000000, -10.00000000000000355 ) ) ;
#9974 = CARTESIAN_POINT ( 'NONE',  ( -5.976238463952679325, 9.000000000000000000, -3.138004751744734477 ) ) ;
#9975 = PRODUCT_DEFINITION_SHAPE ( 'NONE', 'NONE',  #13612 ) ;
#9976 = VECTOR ( 'NONE', #9379, 1000.000000000000000 ) ;
#9977 = DIRECTION ( 'NONE',  ( -0.000000000000000000, -1.000000000000000000, -0.000000000000000000 ) ) ;
#9978 = DIRECTION ( 'NONE',  ( -0.000000000000000000, -1.000000000000000000, -0.000000000000000000 ) ) ;
#9979 = ORIENTED_EDGE ( 'NONE', *, *, #11210, .F. ) ;
#9980 = DIRECTION ( 'NONE',  ( -0.000000000000000000, -1.000000000000000000, -0.000000000000000000 ) ) ;
#9981 = ORIENTED_EDGE ( 'NONE', *, *, #3952, .T. ) ;
#9982 = UNCERTAINTY_MEASURE_WITH_UNIT (LENGTH_MEASURE( 1.000000000000000082E-05 ), #4970, 'distance_accuracy_value', 'NONE');
#9983 = EDGE_LOOP ( 'NONE', ( #9841, #10214, #2256, #6532 ) ) ;
#9984 = CARTESIAN_POINT ( 'NONE',  ( 31.00000000000000000, 0.000000000000000000, 0.000000000000000000 ) ) ;
#9985 = VERTEX_POINT ( 'NONE', #4730 ) ;
#9986 = CIRCLE ( 'NONE', #2954, 1.500000000000003997 ) ;
#9987 = VERTEX_POINT ( 'NONE', #13130 ) ;
#9988 = AXIS2_PLACEMENT_3D ( 'NONE', #7862, #4839, #12083 ) ;
#9989 = CARTESIAN_POINT ( 'NONE',  ( -13.27898586450070084, 0.000000000000000000, -5.170206418547588001 ) ) ;
#9990 = FILL_AREA_STYLE_COLOUR ( '', #9358 ) ;
#9991 = CARTESIAN_POINT ( 'NONE',  ( -12.98835496148321944, 0.000000000000000000, -0.5501230721522551992 ) ) ;
#9992 =( NAMED_UNIT ( * ) PLANE_ANGLE_UNIT ( ) SI_UNIT ( $, .RADIAN. ) );
#9993 = CARTESIAN_POINT ( 'NONE',  ( 31.00000000000000000, 0.09999999999999982514, 3.499999999999999556 ) ) ;
#9994 = CARTESIAN_POINT ( 'NONE',  ( -10.72979803820123479, 0.000000000000000000, -5.571313494980285164 ) ) ;
#9995 = CARTESIAN_POINT ( 'NONE',  ( -5.999999999999991118, 3.000000000000000000, 27.00000000000000000 ) ) ;
#9996 = ORIENTED_EDGE ( 'NONE', *, *, #364, .T. ) ;
#9997 = VECTOR ( 'NONE', #12155, 1000.000000000000000 ) ;
#9998 = CARTESIAN_POINT ( 'NONE',  ( 4.072642252455978884, 3.000000000000000000, 12.14623037080101042 ) ) ;
#9999 = AXIS2_PLACEMENT_3D ( 'NONE', #5518, #10902, #7794 ) ;
#10000 = ADVANCED_BREP_SHAPE_REPRESENTATION ( '', ( #13416, #10007 ), #6493 ) ;
#10001 = VERTEX_POINT ( 'NONE', #1842 ) ;
#10002 = AXIS2_PLACEMENT_3D ( 'NONE', #989, #9390, #8336 ) ;
#10003 = ORIENTED_EDGE ( 'NONE', *, *, #1276, .F. ) ;
#10004 = ORIENTED_EDGE ( 'NONE', *, *, #9593, .T. ) ;
#10005 = EDGE_CURVE ( 'NONE', #8988, #8770, #7149, .T. ) ;
#10006 = CARTESIAN_POINT ( 'NONE',  ( 7.248474140376192310, 9.000000000000000000, 4.439552076088041588 ) ) ;
#10007 = AXIS2_PLACEMENT_3D ( 'NONE', #6754, #3381, #5712 ) ;
#10008 = AXIS2_PLACEMENT_3D ( 'NONE', #7579, #2271, #9704 ) ;
#10009 = DIRECTION ( 'NONE',  ( 0.000000000000000000, 0.000000000000000000, 1.000000000000000000 ) ) ;
#10010 = CARTESIAN_POINT ( 'NONE',  ( 30.73000000000000043, 0.000000000000000000, -2.499999999999995115 ) ) ;
#10011 = DIRECTION ( 'NONE',  ( 0.9254744032703045020, 0.000000000000000000, 0.3788101488760216018 ) ) ;
#10012 = FACE_OUTER_BOUND ( 'NONE', #7121, .T. ) ;
#10013 = CARTESIAN_POINT ( 'NONE',  ( 8.430890348300625448, 3.000000000000000000, 11.48836750521723893 ) ) ;
#10014 = DIRECTION ( 'NONE',  ( -4.625929269271486900E-15, -1.000000000000000000, 0.000000000000000000 ) ) ;
#10015 = DIRECTION ( 'NONE',  ( 0.000000000000000000, 0.000000000000000000, 1.000000000000000000 ) ) ;
#10016 = CARTESIAN_POINT ( 'NONE',  ( 11.13895890373327724, 3.000000000000000000, -7.723663868796764476 ) ) ;
#10017 = DIRECTION ( 'NONE',  ( 0.000000000000000000, 0.000000000000000000, -1.000000000000000000 ) ) ;
#10018 = ORIENTED_EDGE ( 'NONE', *, *, #12580, .T. ) ;
#10019 = VERTEX_POINT ( 'NONE', #6932 ) ;
#10020 = EDGE_CURVE ( 'NONE', #899, #13387, #8110, .T. ) ;
#10021 = EDGE_CURVE ( 'NONE', #9046, #2645, #7334, .T. ) ;
#10022 = VERTEX_POINT ( 'NONE', #6856 ) ;
#10023 = B_SPLINE_CURVE_WITH_KNOTS ( 'NONE', 3,
 ( #370, #302, #12766, #4561 ),
 .UNSPECIFIED., .F., .F.,
 ( 4, 4 ),
 ( 0.000000000000000000, 0.8452273900860258760 ),
 .UNSPECIFIED. ) ;
#10024 = CARTESIAN_POINT ( 'NONE',  ( 0.000000000000000000, 9.000000000000000000, 0.000000000000000000 ) ) ;
#10025 = EDGE_CURVE ( 'NONE', #10192, #11905, #5128, .T. ) ;
#10026 = CARTESIAN_POINT ( 'NONE',  ( -6.660869762029062890, 3.000000000000000000, -11.17001010193236610 ) ) ;
#10027 = EDGE_LOOP ( 'NONE', ( #8106, #2466, #1848, #13202 ) ) ;
#10028 = EDGE_CURVE ( 'NONE', #2208, #10549, #4794, .T. ) ;
#10029 = DIRECTION ( 'NONE',  ( 0.000000000000000000, 1.000000000000000000, -0.000000000000000000 ) ) ;
#10030 = EDGE_CURVE ( 'NONE', #11196, #3596, #4684, .T. ) ;
#10031 = CARTESIAN_POINT ( 'NONE',  ( 0.000000000000000000, 14.00000000000000178, -2.500000000000000000 ) ) ;
#10032 = DIRECTION ( 'NONE',  ( 0.000000000000000000, 1.000000000000000000, 0.000000000000000000 ) ) ;
#10033 = FACE_OUTER_BOUND ( 'NONE', #4458, .T. ) ;
#10034 = CARTESIAN_POINT ( 'NONE',  ( 0.000000000000000000, 3.000000000000000000, 0.000000000000000000 ) ) ;
#10035 = CYLINDRICAL_SURFACE ( 'NONE', #2269, 8.499999999999998224 ) ;
#10036 = EDGE_LOOP ( 'NONE', ( #6276, #12188 ) ) ;
#10037 = EDGE_LOOP ( 'NONE', ( #2203, #8155, #1781, #8022 ) ) ;
#10038 = ORIENTED_EDGE ( 'NONE', *, *, #1095, .F. ) ;
#10039 = CARTESIAN_POINT ( 'NONE',  ( 0.5501230721522984979, 3.000000000000000000, -12.98835496148321766 ) ) ;
#10040 = EDGE_CURVE ( 'NONE', #1280, #12893, #9054, .T. ) ;
#10041 = ORIENTED_EDGE ( 'NONE', *, *, #8298, .T. ) ;
#10042 = CARTESIAN_POINT ( 'NONE',  ( 31.00000000000000000, 3.000000000000000000, -1.600000000000004086 ) ) ;
#10043 = DIRECTION ( 'NONE',  ( 0.5709400946266708354, 1.438358422365572831E-15, 0.8209917224599089236 ) ) ;
#10044 = EDGE_CURVE ( 'NONE', #6718, #10283, #9134, .T. ) ;
#10045 = DIRECTION ( 'NONE',  ( 0.000000000000000000, 1.000000000000000000, 0.000000000000000000 ) ) ;
#10046 = CARTESIAN_POINT ( 'NONE',  ( 29.02231267299996986, 0.000000000000000000, -1.321950885510182250 ) ) ;
#10047 = CARTESIAN_POINT ( 'NONE',  ( -5.830003112347290184, 9.000000000000000000, -5.394061460138155795 ) ) ;
#10048 = DIRECTION ( 'NONE',  ( 0.000000000000000000, 0.000000000000000000, 1.000000000000000000 ) ) ;
#10049 = CARTESIAN_POINT ( 'NONE',  ( 6.000000000000008882, 3.000000000000000000, 27.00000000000000000 ) ) ;
#10050 = VERTEX_POINT ( 'NONE', #5266 ) ;
#10051 = DIRECTION ( 'NONE',  ( 0.000000000000000000, 0.000000000000000000, -1.000000000000000000 ) ) ;
#10052 = ORIENTED_EDGE ( 'NONE', *, *, #11441, .F. ) ;
#10053 = B_SPLINE_SURFACE_WITH_KNOTS ( 'NONE', 3, 1, ( 
 ( #5698, #10560 ),
 ( #11600, #2155 ),
 ( #10634, #3384 ),
 ( #6351, #7597 ) ),
 .UNSPECIFIED., .F., .F., .F.,
 ( 4, 4 ),
 ( 2, 2 ),
 ( 0.1547128134717859205, 1.000000000000000000 ),
 ( 0.000000000000000000, 1.000000000000000000 ),
 .UNSPECIFIED. ) ;
#10054 = ORIENTED_EDGE ( 'NONE', *, *, #6502, .T. ) ;
#10055 = CARTESIAN_POINT ( 'NONE',  ( 7.065816209474156118, 0.000000000000000000, -10.69794375946289833 ) ) ;
#10056 = EDGE_CURVE ( 'NONE', #5504, #7515, #5335, .T. ) ;
#10057 = EDGE_CURVE ( 'NONE', #8568, #13098, #13477, .T. ) ;
#10058 = ORIENTED_EDGE ( 'NONE', *, *, #6082, .T. ) ;
#10059 = CARTESIAN_POINT ( 'NONE',  ( -10.18987059060247624, 0.000000000000000000, -6.506507307819711095 ) ) ;
#10060 = VERTEX_POINT ( 'NONE', #11410 ) ;
#10061 = DIRECTION ( 'NONE',  ( 0.000000000000000000, 0.000000000000000000, -1.000000000000000000 ) ) ;
#10062 =( NAMED_UNIT ( * ) PLANE_ANGLE_UNIT ( ) SI_UNIT ( $, .RADIAN. ) );
#10063 = CARTESIAN_POINT ( 'NONE',  ( -6.217402469309367241, 0.000000000000000000, -13.03533457366727610 ) ) ;
#10064 = CARTESIAN_POINT ( 'NONE',  ( -5.065227977808753224, 0.000000000000000000, -4.461610195077944319 ) ) ;
#10065 = CARTESIAN_POINT ( 'NONE',  ( -0.7527353566742582824, 0.000000000000000000, 7.906594341344654886 ) ) ;
#10066 = CARTESIAN_POINT ( 'NONE',  ( -3.533475733155565290, 9.000000000000000000, 7.730753471893975437 ) ) ;
#10067 = ORIENTED_EDGE ( 'NONE', *, *, #2302, .T. ) ;
#10068 = DIRECTION ( 'NONE',  ( 0.000000000000000000, 0.000000000000000000, 1.000000000000000000 ) ) ;
#10069 = VERTEX_POINT ( 'NONE', #8299 ) ;
#10070 = VECTOR ( 'NONE', #13231, 1000.000000000000000 ) ;
#10071 = VERTEX_POINT ( 'NONE', #6366 ) ;
#10072 = CARTESIAN_POINT ( 'NONE',  ( -10.18979803820068675, 0.000000000000000000, 6.506620931068438196 ) ) ;
#10073 = EDGE_CURVE ( 'NONE', #692, #8710, #8632, .T. ) ;
#10074 = ORIENTED_EDGE ( 'NONE', *, *, #7324, .T. ) ;
#10075 = DIRECTION ( 'NONE',  ( 0.000000000000000000, 0.000000000000000000, 1.000000000000000000 ) ) ;
#10076 = DIRECTION ( 'NONE',  ( -1.000000000000000000, -0.000000000000000000, -0.000000000000000000 ) ) ;
#10077 = DIRECTION ( 'NONE',  ( 0.000000000000000000, 0.000000000000000000, 1.000000000000000000 ) ) ;
#10078 = CARTESIAN_POINT ( 'NONE',  ( -12.25282671965375236, 3.000000000000000000, 5.797378255456025364 ) ) ;
#10079 = CARTESIAN_POINT ( 'NONE',  ( 24.82664254338761722, 3.000000000000000000, 4.561072489069574409 ) ) ;
#10080 = CARTESIAN_POINT ( 'NONE',  ( 9.375397774054407662, 3.000000000000000000, -11.70905276178460497 ) ) ;
#10081 = DIRECTION ( 'NONE',  ( -0.000000000000000000, -1.000000000000000000, -0.000000000000000000 ) ) ;
#10082 = LINE ( 'NONE', #3608, #13226 ) ;
#10083 = DIRECTION ( 'NONE',  ( 0.000000000000000000, 0.000000000000000000, -1.000000000000000000 ) ) ;
#10084 = LINE ( 'NONE', #10152, #8407 ) ;
#10085 = ORIENTED_EDGE ( 'NONE', *, *, #5916, .F. ) ;
#10086 = B_SPLINE_CURVE_WITH_KNOTS ( 'NONE', 3,
 ( #9028, #7122, #386, #4004 ),
 .UNSPECIFIED., .F., .F.,
 ( 4, 4 ),
 ( 0.000000000000000000, 0.8724294488011762327 ),
 .UNSPECIFIED. ) ;
#10087 = VERTEX_POINT ( 'NONE', #8232 ) ;
#10088 = ORIENTED_EDGE ( 'NONE', *, *, #3182, .T. ) ;
#10089 = CYLINDRICAL_SURFACE ( 'NONE', #1171, 2.999999999999999112 ) ;
#10090 = DIRECTION ( 'NONE',  ( -1.000000000000000000, 3.491481338843133355E-15, 2.602085213965210149E-16 ) ) ;
#10091 = CARTESIAN_POINT ( 'NONE',  ( -14.90895795148409420, 3.000000000000000000, 1.650143266773909101 ) ) ;
#10092 = CARTESIAN_POINT ( 'NONE',  ( 0.000000000000000000, 9.000000000000000000, 0.000000000000000000 ) ) ;
#10093 = DIRECTION ( 'NONE',  ( 0.000000000000000000, 0.000000000000000000, 1.000000000000000000 ) ) ;
#10094 = CYLINDRICAL_SURFACE ( 'NONE', #7147, 12.08999999999737618 ) ;
#10095 = LINE ( 'NONE', #12998, #11972 ) ;
#10096 = EDGE_CURVE ( 'NONE', #3304, #10338, #10410, .T. ) ;
#10097 = VERTEX_POINT ( 'NONE', #11612 ) ;
#10098 = ORIENTED_EDGE ( 'NONE', *, *, #4743, .T. ) ;
#10099 = ORIENTED_EDGE ( 'NONE', *, *, #3899, .T. ) ;
#10100 = DIRECTION ( 'NONE',  ( -0.000000000000000000, -1.000000000000000000, -0.000000000000000000 ) ) ;
#10101 = ORIENTED_EDGE ( 'NONE', *, *, #11311, .F. ) ;
#10102 = AXIS2_PLACEMENT_3D ( 'NONE', #13210, #12266, #676 ) ;
#10103 = CARTESIAN_POINT ( 'NONE',  ( 13.04554897075799502, 0.000000000000000000, 5.733772933379473358 ) ) ;
#10104 = CARTESIAN_POINT ( 'NONE',  ( 59.20906036370406156, 31.33135765298363751, 9.098535593462703019 ) ) ;
#10105 = LINE ( 'NONE', #1857, #9477 ) ;
#10106 = CARTESIAN_POINT ( 'NONE',  ( -5.496871281090180972, 0.000000000000000000, 4.899765193453235135 ) ) ;
#10107 = DIRECTION ( 'NONE',  ( -0.000000000000000000, -1.000000000000000000, 0.000000000000000000 ) ) ;
#10108 = EDGE_CURVE ( 'NONE', #10501, #8960, #10576, .T. ) ;
#10109 = DIRECTION ( 'NONE',  ( -0.000000000000000000, -1.000000000000000000, -0.000000000000000000 ) ) ;
#10110 = CARTESIAN_POINT ( 'NONE',  ( -12.98835496148299207, 3.000000000000000000, 0.5501230721524459355 ) ) ;
#10111 = ORIENTED_EDGE ( 'NONE', *, *, #5610, .F. ) ;
#10112 = FACE_OUTER_BOUND ( 'NONE', #1500, .T. ) ;
#10113 = VECTOR ( 'NONE', #8099, 1000.000000000000000 ) ;
#10114 = APPLICATION_CONTEXT ( 'automotive_design' ) ;
#10115 = ORIENTED_EDGE ( 'NONE', *, *, #3634, .T. ) ;
#10116 = CIRCLE ( 'NONE', #11881, 0.1000000000000000472 ) ;
#10117 = UNCERTAINTY_MEASURE_WITH_UNIT (LENGTH_MEASURE( 1.000000000000000082E-05 ), #12492, 'distance_accuracy_value', 'NONE');
#10118 = EDGE_CURVE ( 'NONE', #1088, #8260, #295, .T. ) ;
#10119 = ORIENTED_EDGE ( 'NONE', *, *, #8274, .F. ) ;
#10120 = CARTESIAN_POINT ( 'NONE',  ( -6.506507307819711095, 3.000000000000000000, 10.18987059060247624 ) ) ;
#10121 = EDGE_CURVE ( 'NONE', #3596, #11196, #3804, .T. ) ;
#10122 = ORIENTED_EDGE ( 'NONE', *, *, #12741, .F. ) ;
#10123 = FACE_OUTER_BOUND ( 'NONE', #5261, .T. ) ;
#10124 = ORIENTED_EDGE ( 'NONE', *, *, #12319, .F. ) ;
#10125 = CARTESIAN_POINT ( 'NONE',  ( 2.719999999999997087, 0.000000000000000000, -6.000000000000000000 ) ) ;
#10126 = AXIS2_PLACEMENT_3D ( 'NONE', #9324, #3878, #1055 ) ;
#10127 = CARTESIAN_POINT ( 'NONE',  ( -6.025412986832177076, 3.000000000000000000, -13.73660796332610268 ) ) ;
#10128 = CYLINDRICAL_SURFACE ( 'NONE', #11237, 6.750000000000000888 ) ;
#10129 = CARTESIAN_POINT ( 'NONE',  ( 48.06174015963858892, 0.000000000000000000, -3.086958956539055166 ) ) ;
#10130 = CARTESIAN_POINT ( 'NONE',  ( 2.428572470324196431, 3.000000000000000000, 13.33579367773357127 ) ) ;
#10131 = FACE_OUTER_BOUND ( 'NONE', #8126, .T. ) ;
#10132 = ORIENTED_EDGE ( 'NONE', *, *, #4323, .T. ) ;
#10133 = CARTESIAN_POINT ( 'NONE',  ( 5.517918333394296049, 9.000000000000000000, 4.875228826198821253 ) ) ;
#10134 = ORIENTED_EDGE ( 'NONE', *, *, #1555, .F. ) ;
#10135 = ORIENTED_EDGE ( 'NONE', *, *, #151, .T. ) ;
#10136 = CARTESIAN_POINT ( 'NONE',  ( 0.000000000000000000, 9.000000000000000000, 0.000000000000000000 ) ) ;
#10137 = TOROIDAL_SURFACE ( 'NONE', #10577, 1.600000000000004086, 0.1000000000000000056 ) ;
#10138 = B_SPLINE_SURFACE_WITH_KNOTS ( 'NONE', 3, 1, ( 
 ( #659, #6719 ),
 ( #11962, #2791 ),
 ( #7001, #11197 ),
 ( #2522, #10922 ) ),
 .UNSPECIFIED., .F., .F., .F.,
 ( 4, 4 ),
 ( 2, 2 ),
 ( 0.1547128134717859205, 1.000000000000000000 ),
 ( 0.000000000000000000, 1.000000000000000000 ),
 .UNSPECIFIED. ) ;
#10139 = CIRCLE ( 'NONE', #4416, 3.000000000000000888 ) ;
#10140 = ORIENTED_EDGE ( 'NONE', *, *, #364, .F. ) ;
#10141 = B_SPLINE_CURVE_WITH_KNOTS ( 'NONE', 3,
 ( #3117, #12573, #7205, #7403 ),
 .UNSPECIFIED., .F., .F.,
 ( 4, 4 ),
 ( 0.2727224849193458089, 0.3021405619770169415 ),
 .UNSPECIFIED. ) ;
#10142 = CARTESIAN_POINT ( 'NONE',  ( -0.8123631076467130452, 9.000000000000000000, -6.700937709107179785 ) ) ;
#10143 = DIRECTION ( 'NONE',  ( -0.000000000000000000, -1.000000000000000000, -0.000000000000000000 ) ) ;
#10144 = CARTESIAN_POINT ( 'NONE',  ( -8.180229652970899323, 3.000000000000000000, -11.90209577080756276 ) ) ;
#10145 = CARTESIAN_POINT ( 'NONE',  ( 11.48836750521724070, 3.000000000000000000, -8.430890348300621895 ) ) ;
#10146 = CARTESIAN_POINT ( 'NONE',  ( 52.12339130828321032, 3.000000000000000000, -4.353525159591052685 ) ) ;
#10147 = VECTOR ( 'NONE', #2439, 1000.000000000000000 ) ;
#10148 = ADVANCED_FACE ( 'NONE', ( #7341 ), #12715, .F. ) ;
#10149 = CARTESIAN_POINT ( 'NONE',  ( 3.007863545083557355, 0.000000000000000000, 7.350755164602351677 ) ) ;
#10150 = DIRECTION ( 'NONE',  ( -0.000000000000000000, -1.000000000000000000, -0.000000000000000000 ) ) ;
#10151 = LINE ( 'NONE', #12380, #5137 ) ;
#10152 = CARTESIAN_POINT ( 'NONE',  ( 2.264806262022877714, 3.000000000000000000, -14.82803603298501471 ) ) ;
#10153 = ORIENTED_EDGE ( 'NONE', *, *, #955, .T. ) ;
#10154 = ORIENTED_EDGE ( 'NONE', *, *, #12666, .T. ) ;
#10155 = EDGE_LOOP ( 'NONE', ( #11783, #7208, #8782, #8913 ) ) ;
#10156 = VECTOR ( 'NONE', #4633, 1000.000000000000000 ) ;
#10157 = AXIS2_PLACEMENT_3D ( 'NONE', #2139, #6544, #10744 ) ;
#10158 = ORIENTED_EDGE ( 'NONE', *, *, #8755, .F. ) ;
#10159 = FACE_OUTER_BOUND ( 'NONE', #10918, .T. ) ;
#10160 = SURFACE_STYLE_FILL_AREA ( #4032 ) ;
#10161 = CARTESIAN_POINT ( 'NONE',  ( -11.48836750521723893, 0.000000000000000000, 8.430890348300625448 ) ) ;
#10162 = LINE ( 'NONE', #11200, #12103 ) ;
#10163 = CARTESIAN_POINT ( 'NONE',  ( 0.000000000000000000, 3.000000000000000000, 0.000000000000000000 ) ) ;
#10164 = CIRCLE ( 'NONE', #4441, 9.250000000000000000 ) ;
#10165 = AXIS2_PLACEMENT_3D ( 'NONE', #5652, #1671, #5865 ) ;
#10166 = VECTOR ( 'NONE', #9739, 1000.000000000000000 ) ;
#10167 = CARTESIAN_POINT ( 'NONE',  ( -14.16466328168010769, 3.000000000000000000, -1.557181465540670384 ) ) ;
#10168 = CARTESIAN_POINT ( 'NONE',  ( -0.5398653231797316820, 3.000000000000000000, 12.07794044664754018 ) ) ;
#10169 = ORIENTED_EDGE ( 'NONE', *, *, #2388, .F. ) ;
#10170 = ORIENTED_EDGE ( 'NONE', *, *, #5493, .T. ) ;
#10171 = EDGE_LOOP ( 'NONE', ( #13370, #881, #1570, #8291 ) ) ;
#10172 = FACE_OUTER_BOUND ( 'NONE', #220, .T. ) ;
#10173 = ORIENTED_EDGE ( 'NONE', *, *, #1148, .T. ) ;
#10174 = AXIS2_PLACEMENT_3D ( 'NONE', #8277, #3103, #11446 ) ;
#10175 = AXIS2_PLACEMENT_3D ( 'NONE', #1351, #1491, #9881 ) ;
#10176 = AXIS2_PLACEMENT_3D ( 'NONE', #5951, #1695, #12307 ) ;
#10177 = ADVANCED_FACE ( 'NONE', ( #9265 ), #2233, .F. ) ;
#10178 = DIRECTION ( 'NONE',  ( 0.000000000000000000, 0.000000000000000000, 1.000000000000000000 ) ) ;
#10179 = PRODUCT_DEFINITION ( 'UNKNOWN', '', #12476, #3502 ) ;
#10180 = CARTESIAN_POINT ( 'NONE',  ( 51.42634954137623282, 31.33135765298363040, -11.47886492885842458 ) ) ;
#10181 = CARTESIAN_POINT ( 'NONE',  ( -11.80615107470197778, 3.000000000000000000, -2.604399508763947768 ) ) ;
#10182 = LINE ( 'NONE', #11363, #6384 ) ;
#10183 = DIRECTION ( 'NONE',  ( 0.000000000000000000, 0.000000000000000000, -1.000000000000000000 ) ) ;
#10184 = FACE_OUTER_BOUND ( 'NONE', #9714, .T. ) ;
#10185 = DIRECTION ( 'NONE',  ( 0.000000000000000000, 0.000000000000000000, 1.000000000000000000 ) ) ;
#10186 = ORIENTED_EDGE ( 'NONE', *, *, #6999, .F. ) ;
#10187 = AXIS2_PLACEMENT_3D ( 'NONE', #6733, #3490, #5631 ) ;
#10188 = CARTESIAN_POINT ( 'NONE',  ( 6.736042615721505200, 0.000000000000000000, 5.184180733653466433 ) ) ;
#10189 = CIRCLE ( 'NONE', #3820, 8.500000000000000000 ) ;
#10190 = AXIS2_PLACEMENT_3D ( 'NONE', #10324, #1865, #13501 ) ;
#10191 = ORIENTED_EDGE ( 'NONE', *, *, #9478, .T. ) ;
#10192 = VERTEX_POINT ( 'NONE', #4034 ) ;
#10193 = VERTEX_POINT ( 'NONE', #6236 ) ;
#10194 = CARTESIAN_POINT ( 'NONE',  ( -6.721397655168932062, 9.000000000000000000, 5.203154193476253297 ) ) ;
#10195 = ORIENTED_EDGE ( 'NONE', *, *, #5471, .F. ) ;
#10196 = CARTESIAN_POINT ( 'NONE',  ( -1.650143266773857142, 3.000000000000000000, -14.90895795148409952 ) ) ;
#10197 = EDGE_CURVE ( 'NONE', #9838, #9046, #4164, .T. ) ;
#10198 = ORIENTED_EDGE ( 'NONE', *, *, #5471, .T. ) ;
#10199 = EDGE_CURVE ( 'NONE', #4317, #6406, #1174, .T. ) ;
#10200 = FACE_OUTER_BOUND ( 'NONE', #606, .T. ) ;
#10201 = VECTOR ( 'NONE', #8308, 1000.000000000000000 ) ;
#10202 = PRESENTATION_STYLE_ASSIGNMENT (( #5998 ) ) ;
#10203 = AXIS2_PLACEMENT_3D ( 'NONE', #5177, #906, #13516 ) ;
#10204 = AXIS2_PLACEMENT_3D ( 'NONE', #2063, #2885, #7096 ) ;
#10205 = FACE_OUTER_BOUND ( 'NONE', #2036, .T. ) ;
#10206 = PRESENTATION_STYLE_ASSIGNMENT (( #3994 ) ) ;
#10207 = EDGE_CURVE ( 'NONE', #4297, #746, #5569, .T. ) ;
#10208 = LINE ( 'NONE', #7921, #2503 ) ;
#10209 = EDGE_CURVE ( 'NONE', #4931, #8802, #10642, .T. ) ;
#10210 = CARTESIAN_POINT ( 'NONE',  ( 1.127406311874972422, 0.000000000000000000, -7.862174656777307646 ) ) ;
#10211 = DIRECTION ( 'NONE',  ( 0.000000000000000000, 0.000000000000000000, 1.000000000000000000 ) ) ;
#10212 = VERTEX_POINT ( 'NONE', #10370 ) ;
#10213 = CARTESIAN_POINT ( 'NONE',  ( 30.66173999750687784, 3.000000000000000000, 0.01003121477750366919 ) ) ;
#10214 = ORIENTED_EDGE ( 'NONE', *, *, #1270, .F. ) ;
#10215 = AXIS2_PLACEMENT_3D ( 'NONE', #8236, #13413, #10375 ) ;
#10216 = ORIENTED_EDGE ( 'NONE', *, *, #11300, .T. ) ;
#10217 = VECTOR ( 'NONE', #5655, 1000.000000000000000 ) ;
#10218 = FACE_OUTER_BOUND ( 'NONE', #8289, .T. ) ;
#10219 = EDGE_LOOP ( 'NONE', ( #8500, #5991, #3105, #1016 ) ) ;
#10220 = ADVANCED_FACE ( 'NONE', ( #2040 ), #939, .T. ) ;
#10221 = DIRECTION ( 'NONE',  ( -0.000000000000000000, -1.000000000000000000, -0.000000000000000000 ) ) ;
#10222 = CARTESIAN_POINT ( 'NONE',  ( 11.13895890373327724, 3.000000000000000000, -7.723663868796764476 ) ) ;
#10223 = LINE ( 'NONE', #9447, #5767 ) ;
#10224 = CARTESIAN_POINT ( 'NONE',  ( 0.000000000000000000, 0.000000000000000000, 0.000000000000000000 ) ) ;
#10225 = LINE ( 'NONE', #6024, #9459 ) ;
#10226 = AXIS2_PLACEMENT_3D ( 'NONE', #9262, #13476, #12466 ) ;
#10227 = CARTESIAN_POINT ( 'NONE',  ( -6.217402469309367241, 3.000000000000000000, -13.03533457366727610 ) ) ;
#10228 = CIRCLE ( 'NONE', #1861, 14.25000000000000355 ) ;
#10229 = ADVANCED_FACE ( 'NONE', ( #51 ), #4232, .F. ) ;
#10230 = CARTESIAN_POINT ( 'NONE',  ( 0.000000000000000000, 0.000000000000000000, -5.000000000000000000 ) ) ;
#10231 = FACE_OUTER_BOUND ( 'NONE', #3611, .T. ) ;
#10232 = CARTESIAN_POINT ( 'NONE',  ( 52.12339130828321032, 3.000000000000000000, -4.353525159591052685 ) ) ;
#10233 = DIRECTION ( 'NONE',  ( -0.000000000000000000, -1.000000000000000000, -0.000000000000000000 ) ) ;
#10234 = ORIENTED_EDGE ( 'NONE', *, *, #6115, .T. ) ;
#10235 = ORIENTED_EDGE ( 'NONE', *, *, #10488, .T. ) ;
#10236 = ORIENTED_EDGE ( 'NONE', *, *, #3899, .F. ) ;
#10237 = AXIS2_PLACEMENT_3D ( 'NONE', #11603, #5391, #9658 ) ;
#10238 = EDGE_CURVE ( 'NONE', #5441, #9874, #7410, .T. ) ;
#10239 = EDGE_CURVE ( 'NONE', #4741, #4201, #2490, .T. ) ;
#10240 = ORIENTED_EDGE ( 'NONE', *, *, #6320, .T. ) ;
#10241 = CARTESIAN_POINT ( 'NONE',  ( 51.83140210808490167, 3.000000000000000000, -12.77460472465662988 ) ) ;
#10242 = CARTESIAN_POINT ( 'NONE',  ( 8.883544964651964193, 0.000000000000000000, -12.08646469655236544 ) ) ;
#10243 = DIRECTION ( 'NONE',  ( -0.000000000000000000, -1.000000000000000000, -0.000000000000000000 ) ) ;
#10244 = DIRECTION ( 'NONE',  ( 0.000000000000000000, 1.000000000000000000, 0.000000000000000000 ) ) ;
#10245 = CARTESIAN_POINT ( 'NONE',  ( 5.967832595844252630, 9.000000000000000000, -3.153961652902406154 ) ) ;
#10246 = MECHANICAL_DESIGN_GEOMETRIC_PRESENTATION_REPRESENTATION (  '', ( #8259 ), #4523 ) ;
#10247 = CIRCLE ( 'NONE', #8228, 1.000000000000000888 ) ;
#10248 = CARTESIAN_POINT ( 'NONE',  ( -12.68816982652970893, 3.000000000000000000, 2.830255545554337004 ) ) ;
#10249 = CARTESIAN_POINT ( 'NONE',  ( 0.000000000000000000, 0.000000000000000000, 0.000000000000000000 ) ) ;
#10250 = VERTEX_POINT ( 'NONE', #4511 ) ;
#10251 = CARTESIAN_POINT ( 'NONE',  ( -5.977417671213808070, 9.000000000000000000, 3.135757960025116642 ) ) ;
#10252 = CARTESIAN_POINT ( 'NONE',  ( 4.369710415961185035, 9.000000000000000000, 6.632530905044255576 ) ) ;
#10253 = ORIENTED_EDGE ( 'NONE', *, *, #2278, .T. ) ;
#10254 = CARTESIAN_POINT ( 'NONE',  ( 24.82664254338761722, 3.000000000000000000, 4.561072489069574409 ) ) ;
#10255 = DIRECTION ( 'NONE',  ( 0.5709400946266076637, -9.927781140661384278E-26, 0.8209917224599529995 ) ) ;
#10256 = FACE_OUTER_BOUND ( 'NONE', #6810, .T. ) ;
#10257 = DIRECTION ( 'NONE',  ( -0.000000000000000000, -1.000000000000000000, 0.000000000000000000 ) ) ;
#10258 = LINE ( 'NONE', #5221, #2519 ) ;
#10259 = FACE_OUTER_BOUND ( 'NONE', #12751, .T. ) ;
#10260 = FACE_OUTER_BOUND ( 'NONE', #3612, .T. ) ;
#10261 = VERTEX_POINT ( 'NONE', #2577 ) ;
#10262 = CARTESIAN_POINT ( 'NONE',  ( 7.499999999999999112, 3.000000000000000000, 0.000000000000000000 ) ) ;
#10263 = ORIENTED_EDGE ( 'NONE', *, *, #10883, .T. ) ;
#10264 = PRODUCT_DEFINITION_CONTEXT ( 'detailed design', #7916, 'design' ) ;
#10265 = ORIENTED_EDGE ( 'NONE', *, *, #7592, .T. ) ;
#10266 = ORIENTED_EDGE ( 'NONE', *, *, #2045, .F. ) ;
#10267 = CARTESIAN_POINT ( 'NONE',  ( 0.000000000000000000, 0.000000000000000000, 0.000000000000000000 ) ) ;
#10268 = ORIENTED_EDGE ( 'NONE', *, *, #5555, .F. ) ;
#10269 = DIRECTION ( 'NONE',  ( 0.000000000000000000, 0.000000000000000000, -1.000000000000000000 ) ) ;
#10270 = SHAPE_REPRESENTATION_RELATIONSHIP ( 'NONE' , 'NONE' ,  #6537, #639 ) ;
#10271 = CARTESIAN_POINT ( 'NONE',  ( 1.836970198721030181E-16, 0.000000000000000000, 1.500000000000000222 ) ) ;
#10272 = CYLINDRICAL_SURFACE ( 'NONE', #7706, 0.7499999999999997780 ) ;
#10273 = CYLINDRICAL_SURFACE ( 'NONE', #13293, 14.25000000000000178 ) ;
#10274 = CARTESIAN_POINT ( 'NONE',  ( -8.222660081691577361, 3.000000000000000000, -8.549999999999998934 ) ) ;
#10275 = CARTESIAN_POINT ( 'NONE',  ( 0.000000000000000000, 3.000000000000000000, 0.000000000000000000 ) ) ;
#10276 = ORIENTED_EDGE ( 'NONE', *, *, #4134, .F. ) ;
#10277 = CARTESIAN_POINT ( 'NONE',  ( 48.80418793193314997, 3.000000000000000000, -4.004112872419501201 ) ) ;
#10278 = EDGE_CURVE ( 'NONE', #2558, #5359, #10189, .T. ) ;
#10279 = ORIENTED_EDGE ( 'NONE', *, *, #10901, .T. ) ;
#10280 = EDGE_CURVE ( 'NONE', #912, #5239, #9316, .T. ) ;
#10281 = VERTEX_POINT ( 'NONE', #7670 ) ;
#10282 = LINE ( 'NONE', #11177, #728 ) ;
#10283 = VERTEX_POINT ( 'NONE', #11815 ) ;
#10284 = EDGE_CURVE ( 'NONE', #5247, #2130, #10409, .T. ) ;
#10285 = FACE_BOUND ( 'NONE', #13025, .T. ) ;
#10286 = CARTESIAN_POINT ( 'NONE',  ( 10.67828022838850366, 3.000000000000000000, -7.077546079049271022 ) ) ;
#10287 = DIRECTION ( 'NONE',  ( 0.000000000000000000, 0.000000000000000000, 1.000000000000000000 ) ) ;
#10288 = DIRECTION ( 'NONE',  ( 0.000000000000000000, 0.000000000000000000, 1.000000000000000000 ) ) ;
#10289 = B_SPLINE_CURVE_WITH_KNOTS ( 'NONE', 3,
 ( #1017, #3136, #817, #7349 ),
 .UNSPECIFIED., .F., .F.,
 ( 4, 4 ),
 ( 0.000000000000000000, 0.8452273900860258760 ),
 .UNSPECIFIED. ) ;
#10290 = DIRECTION ( 'NONE',  ( 0.000000000000000000, 0.000000000000000000, -1.000000000000000000 ) ) ;
#10291 = CARTESIAN_POINT ( 'NONE',  ( 41.67875868938293138, 3.000000000000000000, -6.066649533482935119 ) ) ;
#10292 = CARTESIAN_POINT ( 'NONE',  ( 20.00000000000000355, 0.000000000000000000, -14.92471123914604370 ) ) ;
#10293 = DIRECTION ( 'NONE',  ( -0.000000000000000000, -1.000000000000000000, -0.000000000000000000 ) ) ;
#10294 = ORIENTED_EDGE ( 'NONE', *, *, #290, .F. ) ;
#10295 = FACE_OUTER_BOUND ( 'NONE', #3061, .T. ) ;
#10296 = ADVANCED_FACE ( 'NONE', ( #6711 ), #2312, .F. ) ;
#10297 = ORIENTED_EDGE ( 'NONE', *, *, #10096, .F. ) ;
#10298 = VERTEX_POINT ( 'NONE', #8557 ) ;
#10299 = ORIENTED_EDGE ( 'NONE', *, *, #7201, .T. ) ;
#10300 = ADVANCED_FACE ( 'NONE', ( #10651 ), #7858, .T. ) ;
#10301 = ADVANCED_FACE ( 'NONE', ( #7807 ), #3454, .T. ) ;
#10302 = ORIENTED_EDGE ( 'NONE', *, *, #10025, .T. ) ;
#10303 = CARTESIAN_POINT ( 'NONE',  ( 0.000000000000000000, 14.00000000000000178, 0.000000000000000000 ) ) ;
#10304 = CARTESIAN_POINT ( 'NONE',  ( 6.970598036433451661, 0.000000000000000000, -10.97318381393796294 ) ) ;
#10305 = FACE_OUTER_BOUND ( 'NONE', #5784, .T. ) ;
#10306 =( REPRESENTATION_RELATIONSHIP ('NONE','NONE', #3798, #7939 ) REPRESENTATION_RELATIONSHIP_WITH_TRANSFORMATION ( #9807 )SHAPE_REPRESENTATION_RELATIONSHIP( ) );
#10307 = CARTESIAN_POINT ( 'NONE',  ( 0.000000000000000000, 3.000000000000000000, 0.000000000000000000 ) ) ;
#10308 = CARTESIAN_POINT ( 'NONE',  ( 0.000000000000000000, 3.000000000000000000, 0.000000000000000000 ) ) ;
#10309 = ADVANCED_FACE ( 'NONE', ( #12028 ), #11823, .T. ) ;
#10310 = CARTESIAN_POINT ( 'NONE',  ( 46.02418392430381999, 3.000000000000000000, -15.41988256844266658 ) ) ;
#10311 = CARTESIAN_POINT ( 'NONE',  ( -1.105736515254454044, 3.000000000000000000, 13.50994833511691340 ) ) ;
#10312 = ORIENTED_EDGE ( 'NONE', *, *, #5905, .T. ) ;
#10313 = CARTESIAN_POINT ( 'NONE',  ( -6.749999880766614169, 9.000000000000000000, -0.001268720102703135150 ) ) ;
#10314 = CARTESIAN_POINT ( 'NONE',  ( -2.830255545554292151, 0.000000000000000000, -12.68816982652971959 ) ) ;
#10315 = ORIENTED_EDGE ( 'NONE', *, *, #9540, .T. ) ;
#10316 = DIRECTION ( 'NONE',  ( 0.000000000000000000, 0.000000000000000000, 1.000000000000000000 ) ) ;
#10317 = APPLICATION_PROTOCOL_DEFINITION ( 'draft international standard', 'automotive_design', 1998, #7916 ) ;
#10318 = CARTESIAN_POINT ( 'NONE',  ( 0.000000000000000000, 3.000000000000000000, 0.000000000000000000 ) ) ;
#10319 = CARTESIAN_POINT ( 'NONE',  ( 11.70905276178455878, 3.000000000000000000, -9.375397774054460953 ) ) ;
#10320 = CARTESIAN_POINT ( 'NONE',  ( -11.70905276178463872, 3.000000000000000000, -9.375397774054366806 ) ) ;
#10321 = ADVANCED_FACE ( 'NONE', ( #4574 ), #8835, .F. ) ;
#10322 = CARTESIAN_POINT ( 'NONE',  ( -11.52330688609014686, 3.000000000000000000, -6.017756925049552841 ) ) ;
#10323 = EDGE_CURVE ( 'NONE', #1441, #12311, #5462, .T. ) ;
#10324 = CARTESIAN_POINT ( 'NONE',  ( 0.000000000000000000, 9.000000000000000000, 0.000000000000000000 ) ) ;
#10325 = ORIENTED_EDGE ( 'NONE', *, *, #5592, .T. ) ;
#10326 = ORIENTED_EDGE ( 'NONE', *, *, #9565, .F. ) ;
#10327 = CARTESIAN_POINT ( 'NONE',  ( 1.836970198721030181E-16, 3.000000000000000000, 1.500000000000000222 ) ) ;
#10328 = AXIS2_PLACEMENT_3D ( 'NONE', #1368, #4673, #404 ) ;
#10329 = VERTEX_POINT ( 'NONE', #8970 ) ;
#10330 = CARTESIAN_POINT ( 'NONE',  ( 6.736042615721505200, 9.000000000000000000, 5.184180733653466433 ) ) ;
#10331 = CARTESIAN_POINT ( 'NONE',  ( -0.5501230721523990841, 0.000000000000000000, -12.98835496148299384 ) ) ;
#10332 = FACE_OUTER_BOUND ( 'NONE', #9799, .T. ) ;
#10333 = LINE ( 'NONE', #11376, #1635 ) ;
#10334 = AXIS2_PLACEMENT_3D ( 'NONE', #381, #1335, #11876 ) ;
#10335 = DIRECTION ( 'NONE',  ( -0.9248782281665488547, -0.000000000000000000, 0.3802634127332066294 ) ) ;
#10336 = AXIS2_PLACEMENT_3D ( 'NONE', #11453, #6092, #5251 ) ;
#10337 = CARTESIAN_POINT ( 'NONE',  ( 2.264806262022877714, 0.000000000000000000, -14.82803603298501471 ) ) ;
#10338 = VERTEX_POINT ( 'NONE', #11122 ) ;
#10339 = DIRECTION ( 'NONE',  ( 0.000000000000000000, 1.000000000000000000, 0.000000000000000000 ) ) ;
#10340 = ORIENTED_EDGE ( 'NONE', *, *, #12489, .F. ) ;
#10341 = VERTEX_POINT ( 'NONE', #13181 ) ;
#10342 = DIRECTION ( 'NONE',  ( -0.000000000000000000, -1.000000000000000000, 0.000000000000000000 ) ) ;
#10343 = ORIENTED_EDGE ( 'NONE', *, *, #11635, .T. ) ;
#10344 = CIRCLE ( 'NONE', #11888, 0.1000000000000001166 ) ;
#10345 =( GEOMETRIC_REPRESENTATION_CONTEXT ( 3 ) GLOBAL_UNCERTAINTY_ASSIGNED_CONTEXT ( ( #9982 ) ) GLOBAL_UNIT_ASSIGNED_CONTEXT ( ( #4970, #11312, #777 ) ) REPRESENTATION_CONTEXT ( 'NONE', 'WORKASPACE' ) );
#10346 = CARTESIAN_POINT ( 'NONE',  ( -3.469446951953614189E-15, 0.000000000000000000, -6.999999999999998224 ) ) ;
#10347 = CARTESIAN_POINT ( 'NONE',  ( -6.057461899949976747, 0.000000000000000000, 5.137313564148215939 ) ) ;
#10348 = DIRECTION ( 'NONE',  ( 0.000000000000000000, 1.000000000000000000, 0.000000000000000000 ) ) ;
#10349 = CARTESIAN_POINT ( 'NONE',  ( 0.000000000000000000, 0.000000000000000000, 0.000000000000000000 ) ) ;
#10350 = EDGE_CURVE ( 'NONE', #7728, #1004, #6303, .T. ) ;
#10351 = CARTESIAN_POINT ( 'NONE',  ( -5.733772933379472470, 3.000000000000000000, 13.04554897075799502 ) ) ;
#10352 = CONTEXT_DEPENDENT_SHAPE_REPRESENTATION ( #1866, #1510 ) ;
#10353 = DIRECTION ( 'NONE',  ( 0.000000000000000000, 0.000000000000000000, 1.000000000000000000 ) ) ;
#10354 = DIRECTION ( 'NONE',  ( 0.000000000000000000, 1.000000000000000000, 0.000000000000000000 ) ) ;
#10355 = FACE_OUTER_BOUND ( 'NONE', #8599, .T. ) ;
#10356 = CARTESIAN_POINT ( 'NONE',  ( -2.161962830978783057, 0.000000000000000000, -14.08504230442586369 ) ) ;
#10357 = EDGE_LOOP ( 'NONE', ( #8330, #11883 ) ) ;
#10358 = DIRECTION ( 'NONE',  ( -0.000000000000000000, -1.000000000000000000, -0.000000000000000000 ) ) ;
#10359 = AXIS2_PLACEMENT_3D ( 'NONE', #9821, #4451, #6585 ) ;
#10360 = AXIS2_PLACEMENT_3D ( 'NONE', #8113, #1926, #5156 ) ;
#10361 = VERTEX_POINT ( 'NONE', #10013 ) ;
#10362 = ORIENTED_EDGE ( 'NONE', *, *, #3070, .F. ) ;
#10363 = ORIENTED_EDGE ( 'NONE', *, *, #12727, .F. ) ;
#10364 = ORIENTED_EDGE ( 'NONE', *, *, #5729, .T. ) ;
#10365 = CARTESIAN_POINT ( 'NONE',  ( 7.702138240596516638, 0.000000000000000000, -27.99999999999999289 ) ) ;
#10366 = CIRCLE ( 'NONE', #4865, 0.1000000000000000472 ) ;
#10367 = ADVANCED_FACE ( 'NONE', ( #13395 ), #7555, .T. ) ;
#10368 = CIRCLE ( 'NONE', #2225, 8.500000000000001776 ) ;
#10369 = EDGE_CURVE ( 'NONE', #9552, #6730, #6133, .T. ) ;
#10370 = CARTESIAN_POINT ( 'NONE',  ( 19.44487669093179605, 0.000000000000000000, -16.66326752702930847 ) ) ;
#10371 = CARTESIAN_POINT ( 'NONE',  ( 7.146769547044127258, -1.694065894508600678E-18, -1.771712133291270863 ) ) ;
#10372 = DIRECTION ( 'NONE',  ( -0.000000000000000000, 1.000000000000000000, -0.000000000000000000 ) ) ;
#10373 = ADVANCED_FACE ( 'NONE', ( #13256 ), #6680, .T. ) ;
#10374 = EDGE_CURVE ( 'NONE', #12350, #2610, #6455, .T. ) ;
#10375 = DIRECTION ( 'NONE',  ( 0.000000000000000000, 0.000000000000000000, 1.000000000000000000 ) ) ;
#10376 = DIRECTION ( 'NONE',  ( -1.261435711112880913E-16, -0.000000000000000000, -1.000000000000000000 ) ) ;
#10377 = ORIENTED_EDGE ( 'NONE', *, *, #666, .T. ) ;
#10378 = VECTOR ( 'NONE', #4073, 1000.000000000000000 ) ;
#10379 = ORIENTED_EDGE ( 'NONE', *, *, #301, .F. ) ;
#10380 = DIRECTION ( 'NONE',  ( 0.7772490812545874705, 0.000000000000000000, 0.6291930273683107311 ) ) ;
#10381 = ORIENTED_EDGE ( 'NONE', *, *, #11088, .F. ) ;
#10382 = EDGE_CURVE ( 'NONE', #816, #8003, #5465, .T. ) ;
#10383 = CARTESIAN_POINT ( 'NONE',  ( 0.000000000000000000, 13.00000000000000178, -2.500000000000000000 ) ) ;
#10384 = TOROIDAL_SURFACE ( 'NONE', #10604, 3.400000000000001243, 0.1000000000000000056 ) ;
#10385 = SHAPE_DEFINITION_REPRESENTATION ( #10608, #5135 ) ;
#10386 = EDGE_CURVE ( 'NONE', #641, #7781, #13119, .T. ) ;
#10387 = AXIS2_PLACEMENT_3D ( 'NONE', #11154, #11993, #555 ) ;
#10388 = CARTESIAN_POINT ( 'NONE',  ( -6.506620931068619385, 3.000000000000000000, -10.18979803820057306 ) ) ;
#10389 = FACE_OUTER_BOUND ( 'NONE', #10948, .T. ) ;
#10390 = DIRECTION ( 'NONE',  ( 1.000000000000000000, 0.000000000000000000, 1.927470528863118802E-16 ) ) ;
#10391 = EDGE_CURVE ( 'NONE', #6347, #4645, #3154, .T. ) ;
#10392 = CARTESIAN_POINT ( 'NONE',  ( 12.48730470360076161, 3.000000000000000000, -6.329867395090054139 ) ) ;
#10393 = CARTESIAN_POINT ( 'NONE',  ( 2.604399508763944660, 0.000000000000000000, -11.80615107470197600 ) ) ;
#10394 = ORIENTED_EDGE ( 'NONE', *, *, #3165, .T. ) ;
#10395 = VECTOR ( 'NONE', #5246, 1000.000000000000000 ) ;
#10396 = EDGE_LOOP ( 'NONE', ( #8927, #129, #807, #2160 ) ) ;
#10397 = DIRECTION ( 'NONE',  ( -0.6923076923076927347, 0.000000000000000000, 0.7216024245882196597 ) ) ;
#10398 = CIRCLE ( 'NONE', #2915, 3.499999999999999556 ) ;
#10399 = AXIS2_PLACEMENT_3D ( 'NONE', #12222, #12292, #5871 ) ;
#10400 = ORIENTED_EDGE ( 'NONE', *, *, #9370, .T. ) ;
#10401 = B_SPLINE_SURFACE_WITH_KNOTS ( 'NONE', 2, 1, ( 
 ( #2563, #6757 ),
 ( #11168, #9789 ),
 ( #4558, #8745 ) ),
 .UNSPECIFIED., .F., .F., .F.,
 ( 3, 3 ),
 ( 2, 2 ),
 ( 0.000000000000000000, 1.000000000000000000 ),
 ( 0.000000000000000000, 1.000000000000000000 ),
 .UNSPECIFIED. ) ;
#10402 = EDGE_CURVE ( 'NONE', #10019, #3932, #751, .T. ) ;
#10403 = DIRECTION ( 'NONE',  ( 0.000000000000000000, 0.000000000000000000, -1.000000000000000000 ) ) ;
#10404 =( LENGTH_UNIT ( ) NAMED_UNIT ( * ) SI_UNIT ( .MILLI., .METRE. ) );
#10405 = DIRECTION ( 'NONE',  ( 0.000000000000000000, 0.000000000000000000, 1.000000000000000000 ) ) ;
#10406 = CARTESIAN_POINT ( 'NONE',  ( 0.000000000000000000, 3.000000000000000000, 0.000000000000000000 ) ) ;
#10407 = AXIS2_PLACEMENT_3D ( 'NONE', #12805, #10797, #3425 ) ;
#10408 = CARTESIAN_POINT ( 'NONE',  ( -3.893011711613112880, 3.000000000000000000, -12.40340517008282717 ) ) ;
#10409 = B_SPLINE_CURVE_WITH_KNOTS ( 'NONE', 3,
 ( #317, #1271, #7613, #1480 ),
 .UNSPECIFIED., .F., .F.,
 ( 4, 4 ),
 ( 0.000000000000000000, 0.5855695330273008592 ),
 .UNSPECIFIED. ) ;
#10410 = CIRCLE ( 'NONE', #4462, 14.25000000000000178 ) ;
#10411 = VECTOR ( 'NONE', #4275, 1000.000000000000000 ) ;
#10412 = DIRECTION ( 'NONE',  ( 0.000000000000000000, 0.000000000000000000, 1.000000000000000000 ) ) ;
#10413 = CARTESIAN_POINT ( 'NONE',  ( 4.690415759823430619, 3.000000000000000000, 1.399999999999999911 ) ) ;
#10414 = VERTEX_POINT ( 'NONE', #650 ) ;
#10415 = DIRECTION ( 'NONE',  ( 0.000000000000000000, 0.000000000000000000, 1.000000000000000000 ) ) ;
#10416 = ORIENTED_EDGE ( 'NONE', *, *, #5562, .F. ) ;
#10417 = VERTEX_POINT ( 'NONE', #3669 ) ;
#10418 = DIRECTION ( 'NONE',  ( 0.000000000000000000, 0.000000000000000000, 1.000000000000000000 ) ) ;
#10419 = ORIENTED_EDGE ( 'NONE', *, *, #6813, .F. ) ;
#10420 = AXIS2_PLACEMENT_3D ( 'NONE', #13122, #8973, #11260 ) ;
#10421 = AXIS2_PLACEMENT_3D ( 'NONE', #3126, #5064, #3065 ) ;
#10422 = COLOUR_RGB ( '',0.7803921568627451011, 0.7607843137254901578, 0.7411764705882353255 ) ;
#10423 = DIRECTION ( 'NONE',  ( 0.000000000000000000, 0.000000000000000000, 1.000000000000000000 ) ) ;
#10424 = PLANE ( 'NONE',  #560 ) ;
#10425 = CARTESIAN_POINT ( 'NONE',  ( 1.734723475976807094E-15, 2.000000000000000000, 7.000000000000000000 ) ) ;
#10426 = CARTESIAN_POINT ( 'NONE',  ( 8.922226997226882617, 0.000000000000000000, 8.158551673544282679 ) ) ;
#10427 = DIRECTION ( 'NONE',  ( 0.000000000000000000, 0.000000000000000000, 1.000000000000000000 ) ) ;
#10428 = ITEM_DEFINED_TRANSFORMATION ( 'NONE', 'NONE', #6512,  #10007 ) ;
#10429 = CARTESIAN_POINT ( 'NONE',  ( 0.000000000000000000, 3.000000000000000000, 0.000000000000000000 ) ) ;
#10430 = CYLINDRICAL_SURFACE ( 'NONE', #12799, 14.25000000000000000 ) ;
#10431 = CARTESIAN_POINT ( 'NONE',  ( 0.000000000000000000, 0.000000000000000000, 0.000000000000000000 ) ) ;
#10432 = ORIENTED_EDGE ( 'NONE', *, *, #12896, .F. ) ;
#10433 = DIRECTION ( 'NONE',  ( -0.000000000000000000, -1.000000000000000000, -0.000000000000000000 ) ) ;
#10434 = CIRCLE ( 'NONE', #4487, 1.500000000000000222 ) ;
#10435 = EDGE_LOOP ( 'NONE', ( #1378, #5058, #1185, #7263, #10855, #7156 ) ) ;
#10436 = ORIENTED_EDGE ( 'NONE', *, *, #4706, .T. ) ;
#10437 = B_SPLINE_CURVE_WITH_KNOTS ( 'NONE', 3,
 ( #11305, #693, #12347, #1731 ),
 .UNSPECIFIED., .F., .F.,
 ( 4, 4 ),
 ( 0.000000000000000000, 0.5855695330273008592 ),
 .UNSPECIFIED. ) ;
#10438 = EDGE_CURVE ( 'NONE', #12045, #3201, #4035, .T. ) ;
#10439 = VERTEX_POINT ( 'NONE', #5737 ) ;
#10440 = ORIENTED_EDGE ( 'NONE', *, *, #13393, .F. ) ;
#10441 = DIRECTION ( 'NONE',  ( 0.000000000000000000, 0.000000000000000000, 1.000000000000000000 ) ) ;
#10442 = VECTOR ( 'NONE', #7002, 1000.000000000000000 ) ;
#10443 = VECTOR ( 'NONE', #5420, 1000.000000000000000 ) ;
#10444 = FILL_AREA_STYLE_COLOUR ( '', #11987 ) ;
#10445 = AXIS2_PLACEMENT_3D ( 'NONE', #7391, #9518, #6414 ) ;
#10446 = B_SPLINE_CURVE_WITH_KNOTS ( 'NONE', 2,
 ( #7322, #13391, #4015 ),
 .UNSPECIFIED., .F., .F.,
 ( 3, 3 ),
 ( 0.000000000000000000, 1.000000000000000000 ),
 .UNSPECIFIED. ) ;
#10447 = DIRECTION ( 'NONE',  ( 0.000000000000000000, 1.000000000000000000, 0.000000000000000000 ) ) ;
#10448 = CARTESIAN_POINT ( 'NONE',  ( 13.50000000000000355, 0.000000000000000000, -7.050000000000000711 ) ) ;
#10449 = CARTESIAN_POINT ( 'NONE',  ( 41.67875868938293138, 3.000000000000000000, -6.066649533482935119 ) ) ;
#10450 = COLOUR_RGB ( '',0.7803921568627451011, 0.7607843137254901578, 0.7411764705882353255 ) ;
#10451 = VECTOR ( 'NONE', #5452, 1000.000000000000000 ) ;
#10452 = ORIENTED_EDGE ( 'NONE', *, *, #5148, .F. ) ;
#10453 = EDGE_CURVE ( 'NONE', #10888, #12681, #13053, .T. ) ;
#10454 = FACE_OUTER_BOUND ( 'NONE', #9572, .T. ) ;
#10455 = ADVANCED_FACE ( 'NONE', ( #589 ), #9039, .F. ) ;
#10456 = DIRECTION ( 'NONE',  ( -0.000000000000000000, -1.000000000000000000, -0.000000000000000000 ) ) ;
#10457 = ORIENTED_EDGE ( 'NONE', *, *, #7248, .T. ) ;
#10458 = DIRECTION ( 'NONE',  ( 0.000000000000000000, 0.000000000000000000, 1.000000000000000000 ) ) ;
#10459 = EDGE_CURVE ( 'NONE', #2448, #12983, #1040, .T. ) ;
#10460 = CARTESIAN_POINT ( 'NONE',  ( -5.170206418547658167, 3.000000000000000000, -13.27898586450066887 ) ) ;
#10461 = VECTOR ( 'NONE', #8338, 1000.000000000000000 ) ;
#10462 = APPLICATION_PROTOCOL_DEFINITION ( 'draft international standard', 'automotive_design', 1998, #2041 ) ;
#10463 = AXIS2_PLACEMENT_3D ( 'NONE', #11295, #6189, #13366 ) ;
#10464 = CARTESIAN_POINT ( 'NONE',  ( 6.970598036433451661, 3.000000000000000000, -10.97318381393796294 ) ) ;
#10465 = CARTESIAN_POINT ( 'NONE',  ( -6.749999880766614169, 1.734723475976807094E-15, -0.001268720102703522860 ) ) ;
#10466 = DIRECTION ( 'NONE',  ( 0.000000000000000000, 0.000000000000000000, 1.000000000000000000 ) ) ;
#10467 = CARTESIAN_POINT ( 'NONE',  ( -12.40340517008309185, 3.000000000000000000, -3.893011711613028947 ) ) ;
#10468 = CARTESIAN_POINT ( 'NONE',  ( 13.04554897075799502, 3.000000000000000000, 5.733772933379473358 ) ) ;
#10469 = EDGE_CURVE ( 'NONE', #4442, #3224, #11076, .T. ) ;
#10470 = ORIENTED_EDGE ( 'NONE', *, *, #10486, .T. ) ;
#10471 = ORIENTED_EDGE ( 'NONE', *, *, #4253, .F. ) ;
#10472 = AXIS2_PLACEMENT_3D ( 'NONE', #9070, #1653, #1577 ) ;
#10473 = ORIENTED_EDGE ( 'NONE', *, *, #5820, .F. ) ;
#10474 = CARTESIAN_POINT ( 'NONE',  ( 53.04054522416362261, 0.000000000000000000, -3.611077387296437013 ) ) ;
#10475 = ORIENTED_EDGE ( 'NONE', *, *, #6318, .T. ) ;
#10476 = EDGE_CURVE ( 'NONE', #2521, #7249, #5139, .T. ) ;
#10477 = DIRECTION ( 'NONE',  ( -0.000000000000000000, -1.000000000000000000, 0.000000000000000000 ) ) ;
#10478 = CARTESIAN_POINT ( 'NONE',  ( 4.690415759823430619, 3.000000000000000000, 4.500000000000000888 ) ) ;
#10479 = DIRECTION ( 'NONE',  ( -0.000000000000000000, -1.000000000000000000, -0.000000000000000000 ) ) ;
#10480 = AXIS2_PLACEMENT_3D ( 'NONE', #5155, #8445, #1023 ) ;
#10481 = DIRECTION ( 'NONE',  ( -0.000000000000000000, -1.000000000000000000, -0.000000000000000000 ) ) ;
#10482 = CARTESIAN_POINT ( 'NONE',  ( 7.500000000000003553, 3.000000000000000000, 13.39999999999999858 ) ) ;
#10483 = CARTESIAN_POINT ( 'NONE',  ( 31.00000000000000000, 3.000000000000000000, 1.600000000000004086 ) ) ;
#10484 = ORIENTED_EDGE ( 'NONE', *, *, #10601, .T. ) ;
#10485 = DIRECTION ( 'NONE',  ( 0.000000000000000000, 1.000000000000000000, -0.000000000000000000 ) ) ;
#10486 = EDGE_CURVE ( 'NONE', #11304, #5111, #8905, .T. ) ;
#10487 = ORIENTED_EDGE ( 'NONE', *, *, #11889, .T. ) ;
#10488 = EDGE_CURVE ( 'NONE', #5675, #3853, #9537, .T. ) ;
#10489 = ORIENTED_EDGE ( 'NONE', *, *, #5656, .F. ) ;
#10490 = CARTESIAN_POINT ( 'NONE',  ( 2.394769219159762041, 9.000000000000000000, -6.310909632292713844 ) ) ;
#10491 = ORIENTED_EDGE ( 'NONE', *, *, #13345, .F. ) ;
#10492 =( REPRESENTATION_RELATIONSHIP ('NONE','NONE', #3798, #7939 ) REPRESENTATION_RELATIONSHIP_WITH_TRANSFORMATION ( #7669 )SHAPE_REPRESENTATION_RELATIONSHIP( ) );
#10493 = DIRECTION ( 'NONE',  ( 0.000000000000000000, 0.000000000000000000, 1.000000000000000000 ) ) ;
#10494 = CYLINDRICAL_SURFACE ( 'NONE', #9129, 1.000000000000000000 ) ;
#10495 = CARTESIAN_POINT ( 'NONE',  ( 0.000000000000000000, 3.000000000000000000, 0.000000000000000000 ) ) ;
#10496 = CARTESIAN_POINT ( 'NONE',  ( 1.958311002203130480, 3.000000000000000000, -14.87484884897977366 ) ) ;
#10497 = CARTESIAN_POINT ( 'NONE',  ( -12.07793442604884682, 3.000000000000000000, 0.5400000000005513723 ) ) ;
#10498 = DIRECTION ( 'NONE',  ( -0.000000000000000000, -1.000000000000000000, -0.000000000000000000 ) ) ;
#10499 = DIRECTION ( 'NONE',  ( 1.000000000000000000, -3.491481338843133355E-15, 0.000000000000000000 ) ) ;
#10500 = CARTESIAN_POINT ( 'NONE',  ( 9.999999999999992895, -4.163336342344330085E-14, -2.602085213965208275E-15 ) ) ;
#10501 = VERTEX_POINT ( 'NONE', #11396 ) ;
#10502 = CARTESIAN_POINT ( 'NONE',  ( -5.976238463952679325, 9.000000000000000000, -3.138004751744734477 ) ) ;
#10503 = B_SPLINE_SURFACE_WITH_KNOTS ( 'NONE', 3, 1, ( 
 ( #32, #9322 ),
 ( #12509, #5193 ),
 ( #2917, #4209 ),
 ( #9392, #920 ) ),
 .UNSPECIFIED., .F., .F., .F.,
 ( 4, 4 ),
 ( 2, 2 ),
 ( 0.1276832474596253097, 1.000000000000000000 ),
 ( 0.000000000000000000, 1.000000000000000000 ),
 .UNSPECIFIED. ) ;
#10504 = ORIENTED_EDGE ( 'NONE', *, *, #8537, .F. ) ;
#10505 = ADVANCED_FACE ( 'NONE', ( #4213 ), #10561, .T. ) ;
#10506 = ORIENTED_EDGE ( 'NONE', *, *, #5308, .T. ) ;
#10507 = ORIENTED_EDGE ( 'NONE', *, *, #7634, .F. ) ;
#10508 = ORIENTED_EDGE ( 'NONE', *, *, #11927, .T. ) ;
#10509 = DIRECTION ( 'NONE',  ( 0.000000000000000000, 1.000000000000000000, 0.000000000000000000 ) ) ;
#10510 = CARTESIAN_POINT ( 'NONE',  ( 6.217402469309262436, 3.000000000000000000, -13.03533457366732939 ) ) ;
#10511 = CARTESIAN_POINT ( 'NONE',  ( 0.000000000000000000, 3.000000000000000000, 0.000000000000000000 ) ) ;
#10512 = CARTESIAN_POINT ( 'NONE',  ( 31.00000000000000000, 2.900000000000000355, 0.000000000000000000 ) ) ;
#10513 = DIRECTION ( 'NONE',  ( 0.000000000000000000, 0.000000000000000000, 1.000000000000000000 ) ) ;
#10514 = ADVANCED_FACE ( 'NONE', ( #6288 ), #923, .F. ) ;
#10515 = DIRECTION ( 'NONE',  ( 0.000000000000000000, 0.000000000000000000, -1.000000000000000000 ) ) ;
#10516 = VERTEX_POINT ( 'NONE', #7132 ) ;
#10517 = VERTEX_POINT ( 'NONE', #9325 ) ;
#10518 = CARTESIAN_POINT ( 'NONE',  ( 13.50000000000000355, 3.000000000000000000, -7.050000000000000711 ) ) ;
#10519 = ORIENTED_EDGE ( 'NONE', *, *, #5202, .T. ) ;
#10520 = FACE_OUTER_BOUND ( 'NONE', #4772, .T. ) ;
#10521 = PRODUCT_DEFINITION_SHAPE ( 'NONE', 'NONE',  #13620 ) ;
#10522 = CARTESIAN_POINT ( 'NONE',  ( 2.264806262022877714, 3.000000000000000000, -14.82803603298501471 ) ) ;
#10523 = APPLICATION_PROTOCOL_DEFINITION ( 'draft international standard', 'automotive_design', 1998, #713 ) ;
#10524 = CARTESIAN_POINT ( 'NONE',  ( 8.883544964651964193, 3.000000000000000000, -12.08646469655236544 ) ) ;
#10525 = DIRECTION ( 'NONE',  ( -0.000000000000000000, -1.000000000000000000, -0.000000000000000000 ) ) ;
#10526 = EDGE_CURVE ( 'NONE', #6360, #12046, #7397, .T. ) ;
#10527 = EDGE_CURVE ( 'NONE', #8800, #9922, #9880, .T. ) ;
#10528 = LINE ( 'NONE', #11765, #8878 ) ;
#10529 = CARTESIAN_POINT ( 'NONE',  ( 13.04554897075799502, 3.000000000000000000, 5.733772933379473358 ) ) ;
#10530 = CARTESIAN_POINT ( 'NONE',  ( 4.821006024660968947, 3.000000000000000000, -13.61374091949021015 ) ) ;
#10531 = ORIENTED_EDGE ( 'NONE', *, *, #7210, .F. ) ;
#10532 = VERTEX_POINT ( 'NONE', #5317 ) ;
#10533 = ORIENTED_EDGE ( 'NONE', *, *, #113, .T. ) ;
#10534 = CYLINDRICAL_SURFACE ( 'NONE', #13040, 12.08999999999737440 ) ;
#10535 = VERTEX_POINT ( 'NONE', #10291 ) ;
#10536 = DIRECTION ( 'NONE',  ( 0.000000000000000000, 1.000000000000000000, 0.000000000000000000 ) ) ;
#10537 = CYLINDRICAL_SURFACE ( 'NONE', #5779, 1.500000000000003997 ) ;
#10538 = EDGE_CURVE ( 'NONE', #5996, #9693, #11601, .T. ) ;
#10539 = DIRECTION ( 'NONE',  ( 0.000000000000000000, 0.000000000000000000, -1.000000000000000000 ) ) ;
#10540 = EDGE_CURVE ( 'NONE', #594, #3500, #9451, .T. ) ;
#10541 = B_SPLINE_CURVE_WITH_KNOTS ( 'NONE', 3,
 ( #11763, #2329, #1285, #259 ),
 .UNSPECIFIED., .F., .F.,
 ( 4, 4 ),
 ( 0.4545418633443863987, 0.4839599404020549223 ),
 .UNSPECIFIED. ) ;
#10542 = DIRECTION ( 'NONE',  ( 0.000000000000000000, 1.000000000000000000, -0.000000000000000000 ) ) ;
#10543 = EDGE_CURVE ( 'NONE', #8003, #2891, #1958, .T. ) ;
#10544 = CARTESIAN_POINT ( 'NONE',  ( -3.533475733155563070, 0.000000000000000000, 7.730753471893976325 ) ) ;
#10545 = CARTESIAN_POINT ( 'NONE',  ( 11.48836750521724070, 0.000000000000000000, -8.430890348300621895 ) ) ;
#10546 = ORIENTED_EDGE ( 'NONE', *, *, #5019, .T. ) ;
#10547 = EDGE_CURVE ( 'NONE', #8350, #6828, #6766, .T. ) ;
#10548 = DIRECTION ( 'NONE',  ( 0.000000000000000000, 0.000000000000000000, 1.000000000000000000 ) ) ;
#10549 = VERTEX_POINT ( 'NONE', #12638 ) ;
#10550 = EDGE_CURVE ( 'NONE', #4058, #1501, #2716, .T. ) ;
#10551 = ORIENTED_EDGE ( 'NONE', *, *, #11806, .T. ) ;
#10552 = VECTOR ( 'NONE', #9069, 1000.000000000000000 ) ;
#10553 = ORIENTED_EDGE ( 'NONE', *, *, #3633, .T. ) ;
#10554 = CARTESIAN_POINT ( 'NONE',  ( 7.659717769608228366, 9.000000000000000000, -2.099897208369672530 ) ) ;
#10555 = ORIENTED_EDGE ( 'NONE', *, *, #3411, .F. ) ;
#10556 = B_SPLINE_CURVE_WITH_KNOTS ( 'NONE', 3,
 ( #4897, #9097, #778, #7792 ),
 .UNSPECIFIED., .F., .F.,
 ( 4, 4 ),
 ( 0.000000000000000000, 0.8724294488011763438 ),
 .UNSPECIFIED. ) ;
#10557 = CARTESIAN_POINT ( 'NONE',  ( -9.375397774054503586, 3.000000000000000000, -11.70905276178452503 ) ) ;
#10558 = DIRECTION ( 'NONE',  ( 0.000000000000000000, 1.000000000000000000, -0.000000000000000000 ) ) ;
#10559 = CARTESIAN_POINT ( 'NONE',  ( -9.375397774054503586, 0.000000000000000000, -11.70905276178452503 ) ) ;
#10560 = CARTESIAN_POINT ( 'NONE',  ( -2.604399508763953985, 0.000000000000000000, 11.80615107470197778 ) ) ;
#10561 = CYLINDRICAL_SURFACE ( 'NONE', #11299, 1.000000000000000888 ) ;
#10562 = CYLINDRICAL_SURFACE ( 'NONE', #1813, 1.499999999999997780 ) ;
#10563 = CARTESIAN_POINT ( 'NONE',  ( 31.00000000000000000, 3.000000000000000000, 1.499999998612421725 ) ) ;
#10564 = VERTEX_POINT ( 'NONE', #12512 ) ;
#10565 = CARTESIAN_POINT ( 'NONE',  ( 8.883544964651964193, 3.000000000000000000, -12.08646469655236544 ) ) ;
#10566 = ORIENTED_EDGE ( 'NONE', *, *, #10028, .F. ) ;
#10567 = ORIENTED_EDGE ( 'NONE', *, *, #5656, .T. ) ;
#10568 = AXIS2_PLACEMENT_3D ( 'NONE', #3814, #2847, #590 ) ;
#10569 = APPLICATION_CONTEXT ( 'automotive_design' ) ;
#10570 = CIRCLE ( 'NONE', #2863, 12.99999999999977973 ) ;
#10571 = ORIENTED_EDGE ( 'NONE', *, *, #4306, .F. ) ;
#10572 = CARTESIAN_POINT ( 'NONE',  ( 4.201465772524378472, 0.000000000000000000, 6.047394330962382547 ) ) ;
#10573 = CARTESIAN_POINT ( 'NONE',  ( 12.00000000000002132, 8.000000000000000000, -3.122502256758258292E-15 ) ) ;
#10574 = EDGE_CURVE ( 'NONE', #4457, #7143, #997, .T. ) ;
#10575 = ADVANCED_FACE ( 'NONE', ( #8284 ), #8216, .F. ) ;
#10576 = LINE ( 'NONE', #1138, #12179 ) ;
#10577 = AXIS2_PLACEMENT_3D ( 'NONE', #1084, #8251, #7292 ) ;
#10578 = DIRECTION ( 'NONE',  ( 0.000000000000000000, 0.000000000000000000, -1.000000000000000000 ) ) ;
#10579 = DIRECTION ( 'NONE',  ( 0.3788101488760216018, 0.000000000000000000, -0.9254744032703046130 ) ) ;
#10580 = COLOUR_RGB ( '',0.7803921568627451011, 0.7607843137254901578, 0.7411764705882353255 ) ;
#10582 = CARTESIAN_POINT ( 'NONE',  ( -5.170206418547586225, 3.000000000000000000, 13.27898586450069907 ) ) ;
#10581 = B_SPLINE_CURVE_WITH_KNOTS ( 'NONE', 3,
 ( #13514, #8128, #12355, #9376 ),
 .UNSPECIFIED., .F., .F.,
 ( 4, 4 ),
 ( 0.000000000000000000, 0.5855695330273008592 ),
 .UNSPECIFIED. ) ;
#10583 = EDGE_LOOP ( 'NONE', ( #7495, #13173, #4260, #4027 ) ) ;
#10584 = VERTEX_POINT ( 'NONE', #4150 ) ;
#10585 = CARTESIAN_POINT ( 'NONE',  ( 4.369710415961185035, 9.000000000000000000, 6.632530905044255576 ) ) ;
#10586 = VECTOR ( 'NONE', #13022, 1000.000000000000000 ) ;
#10587 = VECTOR ( 'NONE', #13131, 1000.000000000000000 ) ;
#10588 = ORIENTED_EDGE ( 'NONE', *, *, #2874, .T. ) ;
#10589 = DIRECTION ( 'NONE',  ( -0.000000000000000000, -1.000000000000000000, -0.000000000000000000 ) ) ;
#10590 = LINE ( 'NONE', #11485, #12982 ) ;
#10591 = PLANE ( 'NONE',  #11678 ) ;
#10592 = DIRECTION ( 'NONE',  ( -0.000000000000000000, -1.000000000000000000, -0.000000000000000000 ) ) ;
#10593 = CIRCLE ( 'NONE', #6851, 1.000000000000000000 ) ;
#10594 = DIRECTION ( 'NONE',  ( 0.000000000000000000, 1.000000000000000000, 0.000000000000000000 ) ) ;
#10595 = AXIS2_PLACEMENT_3D ( 'NONE', #6401, #8528, #12747 ) ;
#10596 = CARTESIAN_POINT ( 'NONE',  ( 30.79786191028635400, 0.000000000000000000, -6.999232361977355765 ) ) ;
#10597 = EDGE_LOOP ( 'NONE', ( #9627, #11226, #466, #5973 ) ) ;
#10598 = EDGE_LOOP ( 'NONE', ( #1382, #7466 ) ) ;
#10599 = ORIENTED_EDGE ( 'NONE', *, *, #2279, .F. ) ;
#10600 = DIRECTION ( 'NONE',  ( 0.000000000000000000, 0.000000000000000000, 1.000000000000000000 ) ) ;
#10601 = EDGE_CURVE ( 'NONE', #7044, #8783, #311, .T. ) ;
#10602 = ORIENTED_EDGE ( 'NONE', *, *, #3217, .T. ) ;
#10603 = PRODUCT_DEFINITION ( 'UNKNOWN', '', #6960, #10264 ) ;
#10604 = AXIS2_PLACEMENT_3D ( 'NONE', #9352, #6052, #4170 ) ;
#10605 = AXIS2_PLACEMENT_3D ( 'NONE', #1659, #2750, #10048 ) ;
#10606 = CARTESIAN_POINT ( 'NONE',  ( -7.235926821844434365, 0.000000000000000000, 4.459973433655444630 ) ) ;
#10607 =( NAMED_UNIT ( * ) SI_UNIT ( $, .STERADIAN. ) SOLID_ANGLE_UNIT ( ) );
#10608 = PRODUCT_DEFINITION_SHAPE ( 'NONE', 'NONE',  #11618 ) ;
#10609 = FACE_OUTER_BOUND ( 'NONE', #2324, .T. ) ;
#10610 = CARTESIAN_POINT ( 'NONE',  ( 0.000000000000000000, 0.000000000000000000, 0.000000000000000000 ) ) ;
#10611 = CARTESIAN_POINT ( 'NONE',  ( -9.133371500908470608, 0.000000000000000000, -11.90284147956855065 ) ) ;
#10612 = CARTESIAN_POINT ( 'NONE',  ( 2.604531154829233586, 0.000000000000000000, 11.80612203322752585 ) ) ;
#10613 = CARTESIAN_POINT ( 'NONE',  ( -13.61374091949023679, 3.000000000000000000, -4.821006024660923650 ) ) ;
#10614 = ORIENTED_EDGE ( 'NONE', *, *, #6136, .F. ) ;
#10615 = CIRCLE ( 'NONE', #11053, 8.500000000000000000 ) ;
#10616 = CARTESIAN_POINT ( 'NONE',  ( -12.79759916868914615, 3.000000000000000000, -0.7702044561450367421 ) ) ;
#10617 = ORIENTED_EDGE ( 'NONE', *, *, #5906, .F. ) ;
#10618 = AXIS2_PLACEMENT_3D ( 'NONE', #6910, #437, #646 ) ;
#10619 = AXIS2_PLACEMENT_3D ( 'NONE', #3392, #1262, #5454 ) ;
#10620 = ORIENTED_EDGE ( 'NONE', *, *, #13057, .T. ) ;
#10621 = ORIENTED_EDGE ( 'NONE', *, *, #9798, .F. ) ;
#10622 = CARTESIAN_POINT ( 'NONE',  ( 2.525608486058770641, 3.000000000000000000, -2.423076923076923350 ) ) ;
#10623 = ADVANCED_FACE ( 'NONE', ( #13595 ), #6649, .T. ) ;
#10624 = ORIENTED_EDGE ( 'NONE', *, *, #8611, .F. ) ;
#10625 = CARTESIAN_POINT ( 'NONE',  ( 0.6724118135762067183, 3.000000000000000000, -13.82336506795094344 ) ) ;
#10626 = AXIS2_PLACEMENT_3D ( 'NONE', #6177, #13556, #2116 ) ;
#10627 = EDGE_CURVE ( 'NONE', #12193, #3277, #7993, .T. ) ;
#10628 =( NAMED_UNIT ( * ) SI_UNIT ( $, .STERADIAN. ) SOLID_ANGLE_UNIT ( ) );
#10629 = AXIS2_PLACEMENT_3D ( 'NONE', #13407, #12253, #11347 ) ;
#10630 = ADVANCED_FACE ( 'NONE', ( #10758 ), #9749, .T. ) ;
#10631 = VECTOR ( 'NONE', #5438, 1000.000000000000000 ) ;
#10632 = CARTESIAN_POINT ( 'NONE',  ( -14.20034848914876235, 3.000000000000000000, -2.631756770590732764 ) ) ;
#10633 = DIRECTION ( 'NONE',  ( 0.000000000000000000, 0.000000000000000000, 1.000000000000000000 ) ) ;
#10634 = CARTESIAN_POINT ( 'NONE',  ( -2.414978278956346092, 3.000000000000000000, 13.33788847341978467 ) ) ;
#10635 = CARTESIAN_POINT ( 'NONE',  ( -14.20034848914871795, 0.000000000000000000, 2.631756770590945482 ) ) ;
#10636 = CARTESIAN_POINT ( 'NONE',  ( 10.34346111134700585, 3.000000000000000000, 8.760376775873716326 ) ) ;
#10637 = LINE ( 'NONE', #5122, #4292 ) ;
#10638 = ORIENTED_EDGE ( 'NONE', *, *, #8995, .T. ) ;
#10639 = CARTESIAN_POINT ( 'NONE',  ( 5.053288777954491273, 0.000000000000000000, -4.475128213425755952 ) ) ;
#10640 = ORIENTED_EDGE ( 'NONE', *, *, #10056, .F. ) ;
#10641 = ORIENTED_EDGE ( 'NONE', *, *, #737, .F. ) ;
#10642 = CIRCLE ( 'NONE', #10421, 3.100000000000000977 ) ;
#10643 = PRESENTATION_LAYER_ASSIGNMENT (  '', '', ( #9093 ) ) ;
#10644 = ADVANCED_FACE ( 'NONE', ( #3313 ), #6762, .F. ) ;
#10645 = B_SPLINE_CURVE_WITH_KNOTS ( 'NONE', 3,
 ( #1625, #13339, #2786, #7875 ),
 .UNSPECIFIED., .F., .F.,
 ( 4, 4 ),
 ( 0.1276832474596284739, 1.000000000000000000 ),
 .UNSPECIFIED. ) ;
#10646 = ORIENTED_EDGE ( 'NONE', *, *, #10028, .T. ) ;
#10647 = CARTESIAN_POINT ( 'NONE',  ( -5.977417671213808070, 9.000000000000000000, 3.135757960025116642 ) ) ;
#10648 =( LENGTH_UNIT ( ) NAMED_UNIT ( * ) SI_UNIT ( .MILLI., .METRE. ) );
#10649 = EDGE_CURVE ( 'NONE', #7402, #5243, #1194, .T. ) ;
#10650 = CIRCLE ( 'NONE', #12134, 6.749999999999999112 ) ;
#10651 = FACE_OUTER_BOUND ( 'NONE', #3073, .T. ) ;
#10652 = AXIS2_PLACEMENT_3D ( 'NONE', #3717, #1739, #13313 ) ;
#10653 = CARTESIAN_POINT ( 'NONE',  ( 7.499999999999999112, 3.000000000000000000, -1.499999999999997780 ) ) ;
#10654 = CARTESIAN_POINT ( 'NONE',  ( 6.506620931068707314, 0.000000000000000000, 10.18979803820051622 ) ) ;
#10655 = DIRECTION ( 'NONE',  ( -0.000000000000000000, -1.000000000000000000, -0.000000000000000000 ) ) ;
#10656 = ORIENTED_EDGE ( 'NONE', *, *, #4509, .T. ) ;
#10657 = ORIENTED_EDGE ( 'NONE', *, *, #4160, .T. ) ;
#10658 = EDGE_CURVE ( 'NONE', #1111, #13326, #2291, .T. ) ;
#10659 = CARTESIAN_POINT ( 'NONE',  ( 11.11702303352196708, 3.000000000000000000, 8.914835885878218846 ) ) ;
#10660 = ADVANCED_FACE ( 'NONE', ( #10699, #300, #1467, #3248, #8545 ), #1258, .F. ) ;
#10661 = AXIS2_PLACEMENT_3D ( 'NONE', #9757, #12934, #3483 ) ;
#10662 = AXIS2_PLACEMENT_3D ( 'NONE', #6587, #3348, #4326 ) ;
#10663 = VERTEX_POINT ( 'NONE', #6559 ) ;
#10664 = CARTESIAN_POINT ( 'NONE',  ( 2.720000000000001528, 2.000000000000000000, 6.000000000000000000 ) ) ;
#10665 = CARTESIAN_POINT ( 'NONE',  ( 13.50000000000000355, 3.000000000000000000, -5.550000000000001599 ) ) ;
#10666 = CARTESIAN_POINT ( 'NONE',  ( 6.025412986832064277, 3.000000000000000000, -13.73660796332615597 ) ) ;
#10667 = CARTESIAN_POINT ( 'NONE',  ( -0.5400000000007666445, 3.000000000000000000, -12.07793442604883793 ) ) ;
#10668 = PRESENTATION_LAYER_ASSIGNMENT (  '', '', ( #12869 ) ) ;
#10669 = CARTESIAN_POINT ( 'NONE',  ( -13.73660796332618261, 0.000000000000000000, -6.025412986832017204 ) ) ;
#10670 = VECTOR ( 'NONE', #11171, 1000.000000000000000 ) ;
#10671 = DIRECTION ( 'NONE',  ( 0.000000000000000000, 1.000000000000000000, -0.000000000000000000 ) ) ;
#10672 = DIRECTION ( 'NONE',  ( 0.000000000000000000, 0.000000000000000000, -1.000000000000000000 ) ) ;
#10673 = ORIENTED_EDGE ( 'NONE', *, *, #11103, .T. ) ;
#10674 = ORIENTED_EDGE ( 'NONE', *, *, #2483, .T. ) ;
#10675 = EDGE_LOOP ( 'NONE', ( #5482, #6566, #4757, #22 ) ) ;
#10676 = FACE_OUTER_BOUND ( 'NONE', #11580, .T. ) ;
#10677 = EDGE_LOOP ( 'NONE', ( #7590, #3197, #4030, #11078 ) ) ;
#10678 =( GEOMETRIC_REPRESENTATION_CONTEXT ( 3 ) GLOBAL_UNCERTAINTY_ASSIGNED_CONTEXT ( ( #1729 ) ) GLOBAL_UNIT_ASSIGNED_CONTEXT ( ( #103, #7456, #10628 ) ) REPRESENTATION_CONTEXT ( 'NONE', 'WORKASPACE' ) );
#10679 = CARTESIAN_POINT ( 'NONE',  ( 4.690415759823430619, 0.000000000000000000, -4.500000000000000888 ) ) ;
#10680 = SURFACE_SIDE_STYLE ('',( #6471 ) ) ;
#10681 = DIRECTION ( 'NONE',  ( -0.000000000000000000, -1.000000000000000000, -0.000000000000000000 ) ) ;
#10682 = DIRECTION ( 'NONE',  ( 0.000000000000000000, 1.000000000000000000, 0.000000000000000000 ) ) ;
#10683 = DIRECTION ( 'NONE',  ( 0.000000000000000000, 1.000000000000000000, 0.000000000000000000 ) ) ;
#10684 = CARTESIAN_POINT ( 'NONE',  ( -5.299649803506881085, 9.000000000000000000, -6.645578376649351249 ) ) ;
#10685 = CARTESIAN_POINT ( 'NONE',  ( -13.61374091949023679, 0.000000000000000000, -4.821006024660923650 ) ) ;
#10686 = EDGE_CURVE ( 'NONE', #7585, #3491, #8746, .T. ) ;
#10687 = ORIENTED_EDGE ( 'NONE', *, *, #5610, .T. ) ;
#10688 = EDGE_LOOP ( 'NONE', ( #10951, #7664, #2806, #12827 ) ) ;
#10689 = ORIENTED_EDGE ( 'NONE', *, *, #8101, .F. ) ;
#10690 = ORIENTED_EDGE ( 'NONE', *, *, #6604, .F. ) ;
#10691 = PLANE ( 'NONE',  #4895 ) ;
#10692 = ORIENTED_EDGE ( 'NONE', *, *, #5747, .T. ) ;
#10693 = CARTESIAN_POINT ( 'NONE',  ( 7.500000000000003553, 3.000000000000000000, 4.899999999999997691 ) ) ;
#10694 = VERTEX_POINT ( 'NONE', #13591 ) ;
#10695 = DIRECTION ( 'NONE',  ( -1.269138026879196405E-16, 0.000000000000000000, -1.000000000000000000 ) ) ;
#10696 = CYLINDRICAL_SURFACE ( 'NONE', #9731, 1.500000000000001332 ) ;
#10697 = DIRECTION ( 'NONE',  ( -0.000000000000000000, -1.000000000000000000, -0.000000000000000000 ) ) ;
#10698 = CARTESIAN_POINT ( 'NONE',  ( 10.72979803820131472, 3.000000000000000000, 5.571313494980131509 ) ) ;
#10699 = FACE_OUTER_BOUND ( 'NONE', #272, .T. ) ;
#10700 = ADVANCED_FACE ( 'NONE', ( #6625 ), #6428, .F. ) ;
#10701 = CARTESIAN_POINT ( 'NONE',  ( 0.000000000000000000, 0.000000000000000000, 0.000000000000000000 ) ) ;
#10702 = CARTESIAN_POINT ( 'NONE',  ( 0.000000000000000000, 3.000000000000000000, 0.000000000000000000 ) ) ;
#10703 = ADVANCED_FACE ( 'NONE', ( #9595 ), #368, .T. ) ;
#10704 = ORIENTED_EDGE ( 'NONE', *, *, #6528, .T. ) ;
#10705 = DIRECTION ( 'NONE',  ( -0.000000000000000000, -1.000000000000000000, -0.000000000000000000 ) ) ;
#10706 = ORIENTED_EDGE ( 'NONE', *, *, #11873, .T. ) ;
#10707 = ORIENTED_EDGE ( 'NONE', *, *, #5828, .T. ) ;
#10708 = EDGE_CURVE ( 'NONE', #8347, #6705, #11538, .T. ) ;
#10709 = ORIENTED_EDGE ( 'NONE', *, *, #3041, .F. ) ;
#10710 = CARTESIAN_POINT ( 'NONE',  ( 0.5501230721522984979, 0.000000000000000000, -12.98835496148321766 ) ) ;
#10711 = CARTESIAN_POINT ( 'NONE',  ( 6.025412986832064277, 0.000000000000000000, -13.73660796332615597 ) ) ;
#10712 = CARTESIAN_POINT ( 'NONE',  ( -8.369528376005813897, 0.000000000000000000, 1.483574994138652903 ) ) ;
#10713 = EDGE_CURVE ( 'NONE', #5225, #8350, #6696, .T. ) ;
#10714 = CARTESIAN_POINT ( 'NONE',  ( 6.025412986832064277, 3.000000000000000000, -13.73660796332615597 ) ) ;
#10715 = DIRECTION ( 'NONE',  ( 0.000000000000000000, 1.000000000000000000, -0.000000000000000000 ) ) ;
#10716 = DIRECTION ( 'NONE',  ( 0.000000000000000000, 0.000000000000000000, 1.000000000000000000 ) ) ;
#10717 = ORIENTED_EDGE ( 'NONE', *, *, #5309, .T. ) ;
#10718 = EDGE_CURVE ( 'NONE', #12859, #1247, #12905, .T. ) ;
#10719 = EDGE_LOOP ( 'NONE', ( #8615, #7083, #7102, #9081 ) ) ;
#10720 = EDGE_CURVE ( 'NONE', #2149, #868, #4560, .T. ) ;
#10721 = CARTESIAN_POINT ( 'NONE',  ( -5.977417671213808070, 9.000000000000000000, 3.135757960025116642 ) ) ;
#10722 = B_SPLINE_SURFACE_WITH_KNOTS ( 'NONE', 3, 1, ( 
 ( #2620, #4827 ),
 ( #5867, #6822 ),
 ( #7853, #11238 ),
 ( #3864, #1807 ) ),
 .UNSPECIFIED., .F., .F., .F.,
 ( 4, 4 ),
 ( 2, 2 ),
 ( 0.1547128134717859205, 1.000000000000000000 ),
 ( 0.000000000000000000, 1.000000000000000000 ),
 .UNSPECIFIED. ) ;
#10723 = ORIENTED_EDGE ( 'NONE', *, *, #6420, .T. ) ;
#10724 = LINE ( 'NONE', #2385, #1850 ) ;
#10725 = CARTESIAN_POINT ( 'NONE',  ( 0.000000000000000000, 9.000000000000000000, 0.000000000000000000 ) ) ;
#10726 = ADVANCED_FACE ( 'NONE', ( #5387 ), #1414, .T. ) ;
#10727 = LINE ( 'NONE', #7424, #7493 ) ;
#10728 = DIRECTION ( 'NONE',  ( 0.000000000000000000, 0.000000000000000000, 1.000000000000000000 ) ) ;
#10729 = CARTESIAN_POINT ( 'NONE',  ( 30.79786191028635400, 0.000000000000000000, -7.999232361977356653 ) ) ;
#10730 = CARTESIAN_POINT ( 'NONE',  ( 23.99887587215152251, 3.000000000000000000, 5.000000000000000888 ) ) ;
#10731 = SURFACE_STYLE_FILL_AREA ( #8453 ) ;
#10732 = ORIENTED_EDGE ( 'NONE', *, *, #11810, .T. ) ;
#10733 = ORIENTED_EDGE ( 'NONE', *, *, #9282, .T. ) ;
#10734 = VERTEX_POINT ( 'NONE', #634 ) ;
#10735 = ORIENTED_EDGE ( 'NONE', *, *, #490, .T. ) ;
#10736 = CARTESIAN_POINT ( 'NONE',  ( -8.922136023539609440, 0.000000000000000000, 8.158651161643900807 ) ) ;
#10737 = ORIENTED_EDGE ( 'NONE', *, *, #12101, .T. ) ;
#10738 = CARTESIAN_POINT ( 'NONE',  ( 0.000000000000000000, 3.000000000000000000, 0.000000000000000000 ) ) ;
#10739 = EDGE_CURVE ( 'NONE', #5557, #9688, #11536, .T. ) ;
#10740 = DIRECTION ( 'NONE',  ( 0.000000000000000000, 1.000000000000000000, -0.000000000000000000 ) ) ;
#10741 = EDGE_CURVE ( 'NONE', #6705, #916, #6281, .T. ) ;
#10742 = DIRECTION ( 'NONE',  ( 0.000000000000000000, 1.000000000000000000, 0.000000000000000000 ) ) ;
#10743 = CARTESIAN_POINT ( 'NONE',  ( 7.500000000000004441, 3.000000000000000000, 21.89999999999999858 ) ) ;
#10744 = DIRECTION ( 'NONE',  ( 0.000000000000000000, 0.000000000000000000, 1.000000000000000000 ) ) ;
#10745 = DIRECTION ( 'NONE',  ( 0.000000000000000000, 0.000000000000000000, -1.000000000000000000 ) ) ;
#10746 = ORIENTED_EDGE ( 'NONE', *, *, #1733, .T. ) ;
#10747 = LINE ( 'NONE', #159, #9741 ) ;
#10748 = ORIENTED_EDGE ( 'NONE', *, *, #7345, .F. ) ;
#10749 = ORIENTED_EDGE ( 'NONE', *, *, #5475, .T. ) ;
#10750 = AXIS2_PLACEMENT_3D ( 'NONE', #1937, #11307, #9298 ) ;
#10751 = EDGE_LOOP ( 'NONE', ( #6011, #9892, #9255, #9585 ) ) ;
#10752 = CARTESIAN_POINT ( 'NONE',  ( -5.170206418547117266, 0.000000000000000000, 13.27898586450088203 ) ) ;
#10753 = ORIENTED_EDGE ( 'NONE', *, *, #4748, .T. ) ;
#10754 = ORIENTED_EDGE ( 'NONE', *, *, #7588, .T. ) ;
#10755 = DIRECTION ( 'NONE',  ( -0.000000000000000000, -1.000000000000000000, -0.000000000000000000 ) ) ;
#10756 = CARTESIAN_POINT ( 'NONE',  ( -4.334442004268530546, 0.000000000000000000, 7.311813216407585081 ) ) ;
#10757 = CARTESIAN_POINT ( 'NONE',  ( 12.01285915242476499, 3.000000000000000000, -4.000000001073668265 ) ) ;
#10758 = FACE_OUTER_BOUND ( 'NONE', #4391, .T. ) ;
#10759 = CARTESIAN_POINT ( 'NONE',  ( -0.7527353566742582824, 9.000000000000000000, 7.906594341344654886 ) ) ;
#10760 = DIRECTION ( 'NONE',  ( -0.000000000000000000, -1.000000000000000000, -0.000000000000000000 ) ) ;
#10761 = VERTEX_POINT ( 'NONE', #10064 ) ;
#10762 = DIRECTION ( 'NONE',  ( -0.3703953240185315909, 0.000000000000000000, -0.9288742131985401329 ) ) ;
#10763 = ORIENTED_EDGE ( 'NONE', *, *, #13504, .F. ) ;
#10764 = ORIENTED_EDGE ( 'NONE', *, *, #6899, .T. ) ;
#10765 = VERTEX_POINT ( 'NONE', #9993 ) ;
#10766 = CIRCLE ( 'NONE', #7039, 14.25000000000000000 ) ;
#10767 = ADVANCED_FACE ( 'NONE', ( #5929 ), #10722, .F. ) ;
#10768 = CARTESIAN_POINT ( 'NONE',  ( 6.553553527263006551, 9.000000000000000000, 1.616612558808879774 ) ) ;
#10769 = CARTESIAN_POINT ( 'NONE',  ( 7.499999999999999112, 3.000000000000000000, 1.499999999999997780 ) ) ;
#10770 = PRODUCT_CONTEXT ( 'NONE', #10822, 'mechanical' ) ;
#10771 = CARTESIAN_POINT ( 'NONE',  ( 7.940744365623959133, 0.000000000000000000, 0.1715058177969961128 ) ) ;
#10772 = FACE_OUTER_BOUND ( 'NONE', #12816, .T. ) ;
#10773 = LINE ( 'NONE', #6439, #11248 ) ;
#10774 = FACE_OUTER_BOUND ( 'NONE', #10597, .T. ) ;
#10775 = CIRCLE ( 'NONE', #12137, 14.25000000000000000 ) ;
#10776 = VERTEX_POINT ( 'NONE', #10129 ) ;
#10777 = ORIENTED_EDGE ( 'NONE', *, *, #10916, .F. ) ;
#10778 = CARTESIAN_POINT ( 'NONE',  ( 9.600126836553261711, 3.000000000000000000, 8.482622935103766082 ) ) ;
#10779 = EDGE_CURVE ( 'NONE', #9927, #3195, #10208, .T. ) ;
#10780 = VERTEX_POINT ( 'NONE', #13236 ) ;
#10781 = CARTESIAN_POINT ( 'NONE',  ( 24.82664254338761722, 0.000000000000000000, 4.561072489069574409 ) ) ;
#10782 = CARTESIAN_POINT ( 'NONE',  ( 5.967832595844251742, 9.000000000000000000, -3.153961652902404822 ) ) ;
#10783 = EDGE_CURVE ( 'NONE', #12265, #1291, #11749, .T. ) ;
#10784 = CARTESIAN_POINT ( 'NONE',  ( 0.000000000000000000, 3.000000000000000000, 0.000000000000000000 ) ) ;
#10785 = EDGE_CURVE ( 'NONE', #8580, #11681, #8439, .T. ) ;
#10786 = FACE_OUTER_BOUND ( 'NONE', #11020, .T. ) ;
#10787 = CARTESIAN_POINT ( 'NONE',  ( 31.00000000000000000, 2.900000000000000355, 3.499999999999999556 ) ) ;
#10788 = CARTESIAN_POINT ( 'NONE',  ( 0.000000000000000000, 13.00000000000000178, -1.500000000000000222 ) ) ;
#10789 = CARTESIAN_POINT ( 'NONE',  ( -5.797378255456022700, 3.000000000000000000, -12.25282671965375592 ) ) ;
#10790 = CARTESIAN_POINT ( 'NONE',  ( -5.999999999999991118, 0.000000000000000000, 25.50000000000000000 ) ) ;
#10791 = ORIENTED_EDGE ( 'NONE', *, *, #508, .T. ) ;
#10792 = AXIS2_PLACEMENT_3D ( 'NONE', #5910, #13424, #6876 ) ;
#10793 = VERTEX_POINT ( 'NONE', #11026 ) ;
#10794 = VECTOR ( 'NONE', #3769, 1000.000000000000000 ) ;
#10795 = EDGE_LOOP ( 'NONE', ( #467, #7969, #3826, #10624 ) ) ;
#10796 = EDGE_LOOP ( 'NONE', ( #2962, #1884, #7433, #630 ) ) ;
#10797 = DIRECTION ( 'NONE',  ( 0.000000000000000000, 1.000000000000000000, -0.000000000000000000 ) ) ;
#10798 = EDGE_CURVE ( 'NONE', #3116, #12311, #11696, .T. ) ;
#10799 = EDGE_LOOP ( 'NONE', ( #13038, #12892, #12839, #5304 ) ) ;
#10800 = DIRECTION ( 'NONE',  ( -0.000000000000000000, -1.000000000000000000, -0.000000000000000000 ) ) ;
#10801 = EDGE_CURVE ( 'NONE', #2415, #4379, #10556, .T. ) ;
#10802 = AXIS2_PLACEMENT_3D ( 'NONE', #515, #4717, #6289 ) ;
#10803 = DIRECTION ( 'NONE',  ( -0.000000000000000000, -1.000000000000000000, -0.000000000000000000 ) ) ;
#10804 = CARTESIAN_POINT ( 'NONE',  ( -10.72979803820123479, 3.000000000000000000, -5.571313494980285164 ) ) ;
#10805 = CARTESIAN_POINT ( 'NONE',  ( 5.053288777954493050, 9.000000000000000000, -4.475128213425755952 ) ) ;
#10806 = CYLINDRICAL_SURFACE ( 'NONE', #5834, 14.25000000000000000 ) ;
#10807 = ORIENTED_EDGE ( 'NONE', *, *, #2194, .T. ) ;
#10808 = CARTESIAN_POINT ( 'NONE',  ( 2.720000000000001528, 2.000000000000000000, 7.500000000000000888 ) ) ;
#10809 = VERTEX_POINT ( 'NONE', #12009 ) ;
#10810 = ORIENTED_EDGE ( 'NONE', *, *, #3909, .F. ) ;
#10811 = UNCERTAINTY_MEASURE_WITH_UNIT (LENGTH_MEASURE( 1.000000000000000082E-05 ), #11858, 'distance_accuracy_value', 'NONE');
#10812 = VERTEX_POINT ( 'NONE', #7997 ) ;
#10813 = CARTESIAN_POINT ( 'NONE',  ( 2.720000000000001528, 0.000000000000000000, 6.000000000000000000 ) ) ;
#10814 = AXIS2_PLACEMENT_3D ( 'NONE', #1675, #5795, #13105 ) ;
#10815 = ADVANCED_FACE ( 'NONE', ( #702 ), #12073, .F. ) ;
#10816 = ADVANCED_FACE ( 'NONE', ( #12141 ), #4769, .T. ) ;
#10817 = ORIENTED_EDGE ( 'NONE', *, *, #5202, .F. ) ;
#10818 = ORIENTED_EDGE ( 'NONE', *, *, #2310, .T. ) ;
#10819 = CARTESIAN_POINT ( 'NONE',  ( -14.39763212228013955, 3.000000000000000000, -1.133238802859595884 ) ) ;
#10820 = SURFACE_SIDE_STYLE ('',( #9716 ) ) ;
#10821 = EDGE_CURVE ( 'NONE', #9964, #8384, #3163, .T. ) ;
#10822 = APPLICATION_CONTEXT ( 'automotive_design' ) ;
#10823 = DIRECTION ( 'NONE',  ( -1.000000000000000000, -0.000000000000000000, -0.000000000000000000 ) ) ;
#10824 = DIRECTION ( 'NONE',  ( 0.000000000000000000, 1.000000000000000000, 0.000000000000000000 ) ) ;
#10825 = AXIS2_PLACEMENT_3D ( 'NONE', #325, #6646, #4519 ) ;
#10826 = CARTESIAN_POINT ( 'NONE',  ( 2.264806262022877714, 3.000000000000000000, -14.82803603298501471 ) ) ;
#10827 = CIRCLE ( 'NONE', #13264, 0.1000000000000000472 ) ;
#10828 = AXIS2_PLACEMENT_3D ( 'NONE', #7546, #8631, #12980 ) ;
#10829 = CARTESIAN_POINT ( 'NONE',  ( 8.922226997226882617, 3.000000000000000000, 8.158551673544282679 ) ) ;
#10830 = CARTESIAN_POINT ( 'NONE',  ( -4.340891659662447388, 9.000000000000000000, 6.651128039276029469 ) ) ;
#10831 = ORIENTED_EDGE ( 'NONE', *, *, #3303, .T. ) ;
#10832 = DIRECTION ( 'NONE',  ( 0.000000000000000000, 0.000000000000000000, -1.000000000000000000 ) ) ;
#10833 = B_SPLINE_SURFACE_WITH_KNOTS ( 'NONE', 3, 1, ( 
 ( #1468, #5657 ),
 ( #9854, #423 ),
 ( #8808, #3589 ),
 ( #7793, #12011 ) ),
 .UNSPECIFIED., .F., .F., .F.,
 ( 4, 4 ),
 ( 2, 2 ),
 ( 0.000000000000000000, 0.5855695330273008592 ),
 ( 0.000000000000000000, 1.000000000000000000 ),
 .UNSPECIFIED. ) ;
#10834 = B_SPLINE_CURVE_WITH_KNOTS ( 'NONE', 3,
 ( #13135, #9059, #3685, #2732 ),
 .UNSPECIFIED., .F., .F.,
 ( 4, 4 ),
 ( 0.7272709309819391787, 0.7566890080396341256 ),
 .UNSPECIFIED. ) ;
#10835 = EDGE_LOOP ( 'NONE', ( #2394, #6451, #3537, #2165 ) ) ;
#10836 = VERTEX_POINT ( 'NONE', #2564 ) ;
#10837 = AXIS2_PLACEMENT_3D ( 'NONE', #2762, #775, #10403 ) ;
#10838 = VERTEX_POINT ( 'NONE', #13168 ) ;
#10839 = VECTOR ( 'NONE', #12895, 1000.000000000000000 ) ;
#10840 = TOROIDAL_SURFACE ( 'NONE', #4013, 3.399999999999999911, 0.1000000000000000056 ) ;
#10841 = CIRCLE ( 'NONE', #7972, 1.500000000000000222 ) ;
#10842 = CARTESIAN_POINT ( 'NONE',  ( 52.34174591811297717, 3.000000000000000000, -12.24483450274845531 ) ) ;
#10843 = LINE ( 'NONE', #13114, #9997 ) ;
#10844 = CONTEXT_DEPENDENT_SHAPE_REPRESENTATION ( #9157, #5680 ) ;
#10845 = CARTESIAN_POINT ( 'NONE',  ( -8.479748006907129820, 0.000000000000000000, 0.5864074857593144507 ) ) ;
#10846 = FACE_OUTER_BOUND ( 'NONE', #11381, .T. ) ;
#10847 = LINE ( 'NONE', #1214, #13001 ) ;
#10848 = VECTOR ( 'NONE', #10380, 1000.000000000000114 ) ;
#10849 = FACE_OUTER_BOUND ( 'NONE', #9659, .T. ) ;
#10850 = CIRCLE ( 'NONE', #6004, 3.100000000000000533 ) ;
#10851 = ORIENTED_EDGE ( 'NONE', *, *, #12173, .F. ) ;
#10852 = ADVANCED_FACE ( 'NONE', ( #2689 ), #9725, .F. ) ;
#10853 = EDGE_LOOP ( 'NONE', ( #12278, #9514, #5762, #12242 ) ) ;
#10854 = DIRECTION ( 'NONE',  ( -1.000000000000000000, 0.000000000000000000, 0.000000000000000000 ) ) ;
#10855 = ORIENTED_EDGE ( 'NONE', *, *, #2133, .F. ) ;
#10856 = CARTESIAN_POINT ( 'NONE',  ( -14.82803603298502360, 3.000000000000000000, -2.264806262022826644 ) ) ;
#10857 = PRODUCT ( 'base-gear', 'base-gear', '', ( #8310 ) ) ;
#10858 = AXIS2_PLACEMENT_3D ( 'NONE', #3449, #7460, #4421 ) ;
#10859 = DIRECTION ( 'NONE',  ( 0.000000000000000000, 0.000000000000000000, 1.000000000000000000 ) ) ;
#10860 = AXIS2_PLACEMENT_3D ( 'NONE', #1920, #7154, #11414 ) ;
#10861 = FACE_OUTER_BOUND ( 'NONE', #1760, .T. ) ;
#10862 = CARTESIAN_POINT ( 'NONE',  ( 0.8653219153705552502, 0.000000000000000000, -7.312626806738413698 ) ) ;
#10863 = DIRECTION ( 'NONE',  ( -0.000000000000000000, -1.000000000000000000, -0.000000000000000000 ) ) ;
#10864 = DIRECTION ( 'NONE',  ( 0.000000000000000000, 0.000000000000000000, 1.000000000000000000 ) ) ;
#10865 = EDGE_CURVE ( 'NONE', #8366, #1810, #6463, .T. ) ;
#10866 = CARTESIAN_POINT ( 'NONE',  ( 2.830255545554135832, 0.000000000000000000, -12.68816982652952596 ) ) ;
#10867 = ADVANCED_FACE ( 'NONE', ( #5234 ), #2973, .T. ) ;
#10868 = AXIS2_PLACEMENT_3D ( 'NONE', #451, #2588, #8839 ) ;
#10869 = CIRCLE ( 'NONE', #8651, 6.749999999999999112 ) ;
#10870 = EDGE_LOOP ( 'NONE', ( #6780, #3578, #11715, #5852 ) ) ;
#10871 = ORIENTED_EDGE ( 'NONE', *, *, #6899, .F. ) ;
#10872 = ORIENTED_EDGE ( 'NONE', *, *, #1288, .F. ) ;
#10873 = ORIENTED_EDGE ( 'NONE', *, *, #11479, .T. ) ;
#10874 = LINE ( 'NONE', #6595, #2488 ) ;
#10875 = EDGE_CURVE ( 'NONE', #8580, #12645, #10333, .T. ) ;
#10876 = ORIENTED_EDGE ( 'NONE', *, *, #2163, .F. ) ;
#10877 = DIRECTION ( 'NONE',  ( 0.000000000000000000, -0.000000000000000000, -1.000000000000000000 ) ) ;
#10878 = MECHANICAL_DESIGN_GEOMETRIC_PRESENTATION_REPRESENTATION (  '', ( #5378 ), #4940 ) ;
#10879 = AXIS2_PLACEMENT_3D ( 'NONE', #889, #7021, #13425 ) ;
#10880 = CARTESIAN_POINT ( 'NONE',  ( -10.34346111134701118, 0.000000000000000000, -8.760376775873707444 ) ) ;
#10881 = CIRCLE ( 'NONE', #10445, 3.999999999999998224 ) ;
#10882 = LINE ( 'NONE', #11084, #5814 ) ;
#10883 = EDGE_CURVE ( 'NONE', #2378, #10261, #761, .T. ) ;
#10884 = CARTESIAN_POINT ( 'NONE',  ( 8.158551673544288008, 3.000000000000000000, -8.922226997226886169 ) ) ;
#10885 = DIRECTION ( 'NONE',  ( -0.000000000000000000, -1.000000000000000000, -0.000000000000000000 ) ) ;
#10886 = ORIENTED_EDGE ( 'NONE', *, *, #7136, .F. ) ;
#10887 = ORIENTED_EDGE ( 'NONE', *, *, #6101, .F. ) ;
#10888 = VERTEX_POINT ( 'NONE', #975 ) ;
#10889 = FACE_OUTER_BOUND ( 'NONE', #12384, .T. ) ;
#10890 = ADVANCED_FACE ( 'NONE', ( #2007 ), #4565, .F. ) ;
#10891 = VERTEX_POINT ( 'NONE', #4133 ) ;
#10892 = VERTEX_POINT ( 'NONE', #3095 ) ;
#10893 = B_SPLINE_CURVE_WITH_KNOTS ( 'NONE', 3,
 ( #10314, #1923, #3072, #13418 ),
 .UNSPECIFIED., .F., .F.,
 ( 4, 4 ),
 ( 0.5454515525569062495, 0.5748696296145745510 ),
 .UNSPECIFIED. ) ;
#10894 = CARTESIAN_POINT ( 'NONE',  ( 0.7944557581062196006, 9.000000000000000000, -6.703084368289862205 ) ) ;
#10895 = CARTESIAN_POINT ( 'NONE',  ( -13.97385902380755240, 0.000000000000000000, -5.452638258930474713 ) ) ;
#10896 = LINE ( 'NONE', #6971, #894 ) ;
#10897 = COLOUR_RGB ( '',0.7803921568627451011, 0.7607843137254901578, 0.7411764705882353255 ) ;
#10898 = CARTESIAN_POINT ( 'NONE',  ( 1.580708947611199511, 9.000000000000000000, -8.351727918397596540 ) ) ;
#10899 = ADVANCED_FACE ( 'NONE', ( #9302 ), #9227, .T. ) ;
#10900 = DIRECTION ( 'NONE',  ( -0.6204948238377417935, -0.000000000000000000, 0.7842105416216806901 ) ) ;
#10901 = EDGE_CURVE ( 'NONE', #4277, #9276, #13379, .T. ) ;
#10902 = DIRECTION ( 'NONE',  ( -1.000000000000000000, 3.469446951953610639E-15, 2.602085213965210149E-16 ) ) ;
#10903 = ORIENTED_EDGE ( 'NONE', *, *, #565, .F. ) ;
#10904 = CARTESIAN_POINT ( 'NONE',  ( -12.75843939030334795, 0.000000000000000000, 4.577511697546079006 ) ) ;
#10905 = ORIENTED_EDGE ( 'NONE', *, *, #12810, .T. ) ;
#10906 = ORIENTED_EDGE ( 'NONE', *, *, #8021, .T. ) ;
#10907 = EDGE_LOOP ( 'NONE', ( #9709, #12204, #10489, #1019 ) ) ;
#10908 = AXIS2_PLACEMENT_3D ( 'NONE', #10180, #12195, #2745 ) ;
#10909 = DIRECTION ( 'NONE',  ( -0.000000000000000000, -1.000000000000000000, -0.000000000000000000 ) ) ;
#10910 = CARTESIAN_POINT ( 'NONE',  ( 5.571433138827823761, 0.000000000000000000, 10.72973591378220704 ) ) ;
#10911 = DIRECTION ( 'NONE',  ( -0.000000000000000000, -1.000000000000000000, -0.000000000000000000 ) ) ;
#10912 = CARTESIAN_POINT ( 'NONE',  ( 8.795158114916441505, 3.000000000000000000, -9.573149624528689117 ) ) ;
#10913 = EDGE_CURVE ( 'NONE', #11282, #9985, #2282, .T. ) ;
#10914 = CARTESIAN_POINT ( 'NONE',  ( 0.000000000000000000, 0.000000000000000000, 0.000000000000000000 ) ) ;
#10915 = CARTESIAN_POINT ( 'NONE',  ( 1.836970198721030181E-16, 13.00000000000000178, 1.500000000000000222 ) ) ;
#10916 = EDGE_CURVE ( 'NONE', #1554, #76, #10869, .T. ) ;
#10917 = DIRECTION ( 'NONE',  ( -0.000000000000000000, -0.000000000000000000, -1.000000000000000000 ) ) ;
#10918 = EDGE_LOOP ( 'NONE', ( #7469, #1204, #867, #12921 ) ) ;
#10919 = B_SPLINE_CURVE_WITH_KNOTS ( 'NONE', 3,
 ( #4908, #6980, #12225, #11323 ),
 .UNSPECIFIED., .F., .F.,
 ( 4, 4 ),
 ( 0.000000000000000000, 0.8452273900860258760 ),
 .UNSPECIFIED. ) ;
#10920 = ORIENTED_EDGE ( 'NONE', *, *, #4568, .T. ) ;
#10921 = ORIENTED_EDGE ( 'NONE', *, *, #7030, .F. ) ;
#10922 = CARTESIAN_POINT ( 'NONE',  ( -8.914835885878215294, 0.000000000000000000, 11.11702303352197063 ) ) ;
#10923 = FACE_OUTER_BOUND ( 'NONE', #4080, .T. ) ;
#10924 = ADVANCED_FACE ( 'NONE', ( #8268 ), #6310, .F. ) ;
#10925 = CARTESIAN_POINT ( 'NONE',  ( -9.600126836553261711, 3.000000000000000000, -8.482622935103767858 ) ) ;
#10926 = DIRECTION ( 'NONE',  ( 0.000000000000000000, 0.000000000000000000, 1.000000000000000000 ) ) ;
#10927 = CARTESIAN_POINT ( 'NONE',  ( -10.97318381393799136, 3.000000000000000000, -6.970598036433411693 ) ) ;
#10928 = CARTESIAN_POINT ( 'NONE',  ( 12.89546620003432764, 0.000000000000000000, -4.733530556166651415 ) ) ;
#10929 = PLANE ( 'NONE',  #12642 ) ;
#10930 =( NAMED_UNIT ( * ) PLANE_ANGLE_UNIT ( ) SI_UNIT ( $, .RADIAN. ) );
#10931 = ORIENTED_EDGE ( 'NONE', *, *, #7785, .F. ) ;
#10932 = B_SPLINE_SURFACE_WITH_KNOTS ( 'NONE', 2, 1, ( 
 ( #3232, #1173 ),
 ( #1242, #8592 ),
 ( #6475, #215 ) ),
 .UNSPECIFIED., .F., .F., .F.,
 ( 3, 3 ),
 ( 2, 2 ),
 ( 0.000000000000000000, 1.000000000000000000 ),
 ( 0.000000000000000000, 1.000000000000000000 ),
 .UNSPECIFIED. ) ;
#10933 = ORIENTED_EDGE ( 'NONE', *, *, #8252, .T. ) ;
#10934 = ORIENTED_EDGE ( 'NONE', *, *, #9779, .T. ) ;
#10935 = ORIENTED_EDGE ( 'NONE', *, *, #1698, .T. ) ;
#10936 = DIRECTION ( 'NONE',  ( 0.000000000000000000, 0.000000000000000000, -1.000000000000000000 ) ) ;
#10937 = EDGE_LOOP ( 'NONE', ( #13505, #9026, #10268, #1632 ) ) ;
#10938 = EDGE_CURVE ( 'NONE', #10985, #11917, #6201, .T. ) ;
#10939 = DIRECTION ( 'NONE',  ( 0.000000000000000000, 0.000000000000000000, 1.000000000000000000 ) ) ;
#10940 = PRODUCT_DEFINITION ( 'UNKNOWN', '', #2999, #6686 ) ;
#10941 =( NAMED_UNIT ( * ) SI_UNIT ( $, .STERADIAN. ) SOLID_ANGLE_UNIT ( ) );
#10942 = B_SPLINE_SURFACE_WITH_KNOTS ( 'NONE', 3, 1, ( 
 ( #6839, #5807 ),
 ( #4780, #1751 ),
 ( #10144, #3601 ),
 ( #4914, #8967 ) ),
 .UNSPECIFIED., .F., .F., .F.,
 ( 4, 4 ),
 ( 2, 2 ),
 ( 0.000000000000000000, 0.5855695330273008592 ),
 ( 0.000000000000000000, 1.000000000000000000 ),
 .UNSPECIFIED. ) ;
#10943 = CARTESIAN_POINT ( 'NONE',  ( 12.63269908545826503, 0.000000000000000000, -5.340493616518841691 ) ) ;
#10944 = PLANE ( 'NONE',  #1334 ) ;
#10945 = DIRECTION ( 'NONE',  ( 0.000000000000000000, 1.000000000000000000, 0.000000000000000000 ) ) ;
#10946 = LINE ( 'NONE', #12124, #1367 ) ;
#10947 = CARTESIAN_POINT ( 'NONE',  ( 3.555260608155774271, 9.000000000000000000, 7.720759160088842776 ) ) ;
#10948 = EDGE_LOOP ( 'NONE', ( #11802, #1075, #5797, #7583 ) ) ;
#10949 = CARTESIAN_POINT ( 'NONE',  ( -2.631756770590896632, 0.000000000000000000, -14.20034848914872505 ) ) ;
#10950 = ORIENTED_EDGE ( 'NONE', *, *, #13327, .T. ) ;
#10951 = ORIENTED_EDGE ( 'NONE', *, *, #3046, .T. ) ;
#10952 = FACE_OUTER_BOUND ( 'NONE', #3253, .T. ) ;
#10953 = ORIENTED_EDGE ( 'NONE', *, *, #9632, .F. ) ;
#10954 = EDGE_CURVE ( 'NONE', #4645, #13453, #8130, .T. ) ;
#10955 = ORIENTED_EDGE ( 'NONE', *, *, #1796, .F. ) ;
#10956 = ADVANCED_FACE ( 'NONE', ( #7306 ), #10273, .T. ) ;
#10957 = DIRECTION ( 'NONE',  ( 0.000000000000000000, 0.000000000000000000, 1.000000000000000000 ) ) ;
#10958 = CARTESIAN_POINT ( 'NONE',  ( -6.017756925049793537, 0.000000000000000000, -11.52330688609026232 ) ) ;
#10959 = LINE ( 'NONE', #5866, #3522 ) ;
#10960 = ADVANCED_FACE ( 'NONE', ( #3995 ), #12689, .T. ) ;
#10961 = CARTESIAN_POINT ( 'NONE',  ( 31.00000000000000000, 0.09999999999999982514, 1.600000000000004086 ) ) ;
#10962 = EDGE_CURVE ( 'NONE', #4201, #4741, #11965, .T. ) ;
#10963 = CARTESIAN_POINT ( 'NONE',  ( -11.46847481510586775, 0.000000000000000000, -5.708888906988912382 ) ) ;
#10964 = CARTESIAN_POINT ( 'NONE',  ( -2.161962830978702677, 0.000000000000000000, 14.08504230442587435 ) ) ;
#10965 = EDGE_LOOP ( 'NONE', ( #7509, #10294, #4095, #4946 ) ) ;
#10966 = DIRECTION ( 'NONE',  ( 0.000000000000000000, 1.000000000000000000, 0.000000000000000000 ) ) ;
#10967 = ORIENTED_EDGE ( 'NONE', *, *, #8053, .F. ) ;
#10968 = PRODUCT_DEFINITION_SHAPE ( 'NONE', 'NONE',  #13613 ) ;
#10969 = ORIENTED_EDGE ( 'NONE', *, *, #13230, .F. ) ;
#10970 = ORIENTED_EDGE ( 'NONE', *, *, #4202, .T. ) ;
#10971 = EDGE_CURVE ( 'NONE', #11905, #11924, #2197, .T. ) ;
#10972 = CARTESIAN_POINT ( 'NONE',  ( 12.03251085770905959, 3.000000000000000000, 3.999999998926332179 ) ) ;
#10973 = CARTESIAN_POINT ( 'NONE',  ( 1.836970198721030181E-16, 3.000000000000000000, 1.500000000000000222 ) ) ;
#10974 = CARTESIAN_POINT ( 'NONE',  ( -8.771102293099080072, 0.000000000000000000, -10.33484986938307770 ) ) ;
#10975 = CARTESIAN_POINT ( 'NONE',  ( -1.133238802859761973, 0.000000000000000000, -14.39763212228013067 ) ) ;
#10976 = ITEM_DEFINED_TRANSFORMATION ( 'NONE', 'NONE', #3863,  #10007 ) ;
#10977 = DIRECTION ( 'NONE',  ( 0.000000000000000000, 1.000000000000000000, -0.000000000000000000 ) ) ;
#10978 = CARTESIAN_POINT ( 'NONE',  ( 0.000000000000000000, 3.000000000000000000, 0.000000000000000000 ) ) ;
#10979 = CARTESIAN_POINT ( 'NONE',  ( 3.555260608155774271, 9.000000000000000000, 7.720759160088842776 ) ) ;
#10980 = CYLINDRICAL_SURFACE ( 'NONE', #80, 6.750000000000000888 ) ;
#10981 = ORIENTED_EDGE ( 'NONE', *, *, #13300, .F. ) ;
#10982 = EDGE_LOOP ( 'NONE', ( #4396, #12079, #3898, #13204 ) ) ;
#10983 = AXIS2_PLACEMENT_3D ( 'NONE', #9148, #615, #10316 ) ;
#10984 = EDGE_CURVE ( 'NONE', #594, #8041, #11085, .T. ) ;
#10985 = VERTEX_POINT ( 'NONE', #8525 ) ;
#10986 = LINE ( 'NONE', #5958, #4033 ) ;
#10987 = CARTESIAN_POINT ( 'NONE',  ( 7.500000000000003553, 0.000000000000000000, 13.39999999999999858 ) ) ;
#10988 = DIRECTION ( 'NONE',  ( 0.000000000000000000, 0.000000000000000000, -1.000000000000000000 ) ) ;
#10989 = AXIS2_PLACEMENT_3D ( 'NONE', #10448, #8496, #3205 ) ;
#10990 = CARTESIAN_POINT ( 'NONE',  ( 5.280889752749253319, 0.000000000000000000, -6.660495733750448899 ) ) ;
#10991 = CARTESIAN_POINT ( 'NONE',  ( 6.660877044263387781, 0.000000000000000000, -11.16999893002129696 ) ) ;
#10992 = AXIS2_PLACEMENT_3D ( 'NONE', #10349, #2021, #10288 ) ;
#10993 = FACE_OUTER_BOUND ( 'NONE', #9494, .T. ) ;
#10994 = CARTESIAN_POINT ( 'NONE',  ( 0.000000000000000000, 13.00000000000000178, 0.000000000000000000 ) ) ;
#10995 = DIRECTION ( 'NONE',  ( -0.000000000000000000, -1.000000000000000000, -0.000000000000000000 ) ) ;
#10996 = EDGE_LOOP ( 'NONE', ( #13324, #1763, #5519, #5904 ) ) ;
#10997 = ORIENTED_EDGE ( 'NONE', *, *, #13353, .F. ) ;
#10998 = ORIENTED_EDGE ( 'NONE', *, *, #12268, .T. ) ;
#10999 = DIRECTION ( 'NONE',  ( 0.000000000000000000, 0.000000000000000000, -1.000000000000000000 ) ) ;
#11000 = AXIS2_PLACEMENT_3D ( 'NONE', #9900, #3637, #12053 ) ;
#11001 =( REPRESENTATION_RELATIONSHIP ('NONE','NONE', #3798, #8461 ) REPRESENTATION_RELATIONSHIP_WITH_TRANSFORMATION ( #2024 )SHAPE_REPRESENTATION_RELATIONSHIP( ) );
#11002 = CIRCLE ( 'NONE', #5068, 14.25000000000000178 ) ;
#11003 = ORIENTED_EDGE ( 'NONE', *, *, #13136, .F. ) ;
#11004 = B_SPLINE_CURVE_WITH_KNOTS ( 'NONE', 3,
 ( #755, #8993, #8111, #1925 ),
 .UNSPECIFIED., .F., .F.,
 ( 4, 4 ),
 ( 0.000000000000000000, 0.8452273900860258760 ),
 .UNSPECIFIED. ) ;
#11005 = FACE_BOUND ( 'NONE', #6791, .T. ) ;
#11006 = DIRECTION ( 'NONE',  ( 0.3534274726160315794, 1.141457706935629186E-21, -0.9354619295301355164 ) ) ;
#11007 = CYLINDRICAL_SURFACE ( 'NONE', #6178, 6.750000000000000888 ) ;
#11008 = CARTESIAN_POINT ( 'NONE',  ( 4.690415759823430619, 0.09999999999999982514, -4.500000000000000888 ) ) ;
#11009 = CARTESIAN_POINT ( 'NONE',  ( -5.250000000000000000, 3.000000000000000000, -26.44078293894052578 ) ) ;
#11010 = CIRCLE ( 'NONE', #40, 14.25000000000000178 ) ;
#11011 = CARTESIAN_POINT ( 'NONE',  ( 0.000000000000000000, 3.000000000000000000, 0.000000000000000000 ) ) ;
#11012 = VECTOR ( 'NONE', #11829, 1000.000000000000000 ) ;
#11013 = DIRECTION ( 'NONE',  ( 0.000000000000000000, 0.000000000000000000, 1.000000000000000000 ) ) ;
#11014 = ORIENTED_EDGE ( 'NONE', *, *, #12522, .T. ) ;
#11015 = CARTESIAN_POINT ( 'NONE',  ( -8.352599575481690408, 3.000000000000000000, 30.99999999999999289 ) ) ;
#11016 = VERTEX_POINT ( 'NONE', #12745 ) ;
#11017 = EDGE_CURVE ( 'NONE', #3089, #655, #2265, .T. ) ;
#11018 = ORIENTED_EDGE ( 'NONE', *, *, #2072, .T. ) ;
#11019 = DIRECTION ( 'NONE',  ( 0.000000000000000000, 0.000000000000000000, 1.000000000000000000 ) ) ;
#11020 = EDGE_LOOP ( 'NONE', ( #789, #4974, #3868, #6280 ) ) ;
#11021 = TOROIDAL_SURFACE ( 'NONE', #2015, 3.100000000000000977, 0.1000000000000000056 ) ;
#11022 = ORIENTED_EDGE ( 'NONE', *, *, #5820, .T. ) ;
#11023 = DIRECTION ( 'NONE',  ( 0.000000000000000000, 0.000000000000000000, 1.000000000000000000 ) ) ;
#11024 = DIRECTION ( 'NONE',  ( -1.000000000000000000, -0.000000000000000000, 1.055752450943286591E-16 ) ) ;
#11025 = CARTESIAN_POINT ( 'NONE',  ( 0.7901945867173618687, 3.000000000000000000, 12.78643498603817541 ) ) ;
#11026 = CARTESIAN_POINT ( 'NONE',  ( 13.04554897075799502, 3.000000000000000000, 5.733772933379473358 ) ) ;
#11027 = CARTESIAN_POINT ( 'NONE',  ( -5.975392301194336397, 9.000000000000000000, -6.045220165289885372 ) ) ;
#11028 = LINE ( 'NONE', #8955, #784 ) ;
#11029 = ORIENTED_EDGE ( 'NONE', *, *, #2874, .F. ) ;
#11030 = CARTESIAN_POINT ( 'NONE',  ( -6.721397655168932062, 9.000000000000000000, 5.203154193476253297 ) ) ;
#11031 = CIRCLE ( 'NONE', #4873, 2.999999999999999112 ) ;
#11032 = ADVANCED_FACE ( 'NONE', ( #9637 ), #154, .F. ) ;
#11033 = VERTEX_POINT ( 'NONE', #1241 ) ;
#11034 = EDGE_CURVE ( 'NONE', #4686, #2755, #5802, .T. ) ;
#11035 = ORIENTED_EDGE ( 'NONE', *, *, #5031, .F. ) ;
#11036 = ORIENTED_EDGE ( 'NONE', *, *, #8687, .F. ) ;
#11037 = EDGE_CURVE ( 'NONE', #6668, #5900, #9052, .T. ) ;
#11038 = EDGE_CURVE ( 'NONE', #3932, #1933, #5299, .T. ) ;
#11039 = CARTESIAN_POINT ( 'NONE',  ( 2.719999999999997087, 2.000000000000000000, -6.000000000000000000 ) ) ;
#11040 = VECTOR ( 'NONE', #13485, 1000.000000000000000 ) ;
#11041 = CARTESIAN_POINT ( 'NONE',  ( 0.5501230721522984979, 3.000000000000000000, -12.98835496148321766 ) ) ;
#11042 = CARTESIAN_POINT ( 'NONE',  ( -13.82336506795071607, 3.000000000000000000, 0.6724118135763649251 ) ) ;
#11043 = CARTESIAN_POINT ( 'NONE',  ( -3.833392836528145331, 1.734723475976807094E-15, -5.555861711818853799 ) ) ;
#11044 = DIRECTION ( 'NONE',  ( 0.000000000000000000, 0.000000000000000000, -1.000000000000000000 ) ) ;
#11045 = CONTEXT_DEPENDENT_SHAPE_REPRESENTATION ( #10306, #9638 ) ;
#11046 = DIRECTION ( 'NONE',  ( -0.000000000000000000, -1.000000000000000000, -0.000000000000000000 ) ) ;
#11047 = CARTESIAN_POINT ( 'NONE',  ( 19.60942157306000766, 0.000000000000000000, 14.05941790610251374 ) ) ;
#11048 = FACE_OUTER_BOUND ( 'NONE', #6014, .T. ) ;
#11049 = CARTESIAN_POINT ( 'NONE',  ( 10.67828022838850366, 3.000000000000000000, -7.077546079049271022 ) ) ;
#11050 = DIRECTION ( 'NONE',  ( -1.000000000000000000, 0.000000000000000000, 9.145772869372436484E-17 ) ) ;
#11051 = EDGE_CURVE ( 'NONE', #3124, #9464, #4541, .T. ) ;
#11052 = ORIENTED_EDGE ( 'NONE', *, *, #7467, .T. ) ;
#11053 = AXIS2_PLACEMENT_3D ( 'NONE', #13372, #832, #11019 ) ;
#11054 = ORIENTED_EDGE ( 'NONE', *, *, #5240, .F. ) ;
#11055 = VECTOR ( 'NONE', #10433, 1000.000000000000000 ) ;
#11056 = PRODUCT_DEFINITION_SHAPE ( 'NONE', 'NONE',  #5706 ) ;
#11057 = EDGE_CURVE ( 'NONE', #5801, #3370, #9332, .T. ) ;
#11058 = ORIENTED_EDGE ( 'NONE', *, *, #986, .T. ) ;
#11059 = CARTESIAN_POINT ( 'NONE',  ( 53.04054522416362261, 3.000000000000000000, -3.611077387296437013 ) ) ;
#11060 = CARTESIAN_POINT ( 'NONE',  ( 0.000000000000000000, 3.000000000000000000, -5.000000000000000000 ) ) ;
#11061 = AXIS2_PLACEMENT_3D ( 'NONE', #12327, #10100, #7890 ) ;
#11062 = FACE_OUTER_BOUND ( 'NONE', #12624, .T. ) ;
#11063 = VECTOR ( 'NONE', #4934, 1000.000000000000000 ) ;
#11064 = AXIS2_PLACEMENT_3D ( 'NONE', #11516, #8135, #8273 ) ;
#11065 = CARTESIAN_POINT ( 'NONE',  ( 5.280889752749253319, 9.000000000000000000, -6.660495733750448899 ) ) ;
#11066 = CARTESIAN_POINT ( 'NONE',  ( 6.017756925049591921, 0.000000000000000000, -11.52330688609011844 ) ) ;
#11067 = DIRECTION ( 'NONE',  ( 0.000000000000000000, 0.000000000000000000, 1.000000000000000000 ) ) ;
#11068 = CARTESIAN_POINT ( 'NONE',  ( 3.893011711613070691, 0.000000000000000000, -12.40340517008307231 ) ) ;
#11069 = EDGE_CURVE ( 'NONE', #843, #4282, #10434, .T. ) ;
#11070 = CARTESIAN_POINT ( 'NONE',  ( -13.17831234185052836, 3.000000000000000000, -4.227250083625696320 ) ) ;
#11071 = ORIENTED_EDGE ( 'NONE', *, *, #130, .T. ) ;
#11072 = ORIENTED_EDGE ( 'NONE', *, *, #1993, .F. ) ;
#11073 = ORIENTED_EDGE ( 'NONE', *, *, #7340, .F. ) ;
#11074 = AXIS2_PLACEMENT_3D ( 'NONE', #2587, #6782, #9132 ) ;
#11075 = CARTESIAN_POINT ( 'NONE',  ( -13.28140389626389783, 0.000000000000000000, -1.567980996311402420 ) ) ;
#11076 = CIRCLE ( 'NONE', #9967, 12.08999999999737440 ) ;
#11077 = AXIS2_PLACEMENT_3D ( 'NONE', #3485, #3625, #6661 ) ;
#11078 = ORIENTED_EDGE ( 'NONE', *, *, #13096, .T. ) ;
#11079 = CYLINDRICAL_SURFACE ( 'NONE', #7470, 1.000000000000000888 ) ;
#11080 = DIRECTION ( 'NONE',  ( -0.3537595828326807190, 1.222174860403972347E-21, -0.9353363873783847593 ) ) ;
#11081 = DIRECTION ( 'NONE',  ( 0.000000000000000000, 0.000000000000000000, 1.000000000000000000 ) ) ;
#11082 = CARTESIAN_POINT ( 'NONE',  ( 26.30958424017656938, 0.09999999999999982514, -1.500000000000000000 ) ) ;
#11083 = CIRCLE ( 'NONE', #8864, 1.500000000000001332 ) ;
#11084 = CARTESIAN_POINT ( 'NONE',  ( -21.21140389626389577, 0.000000000000000000, -14.83930531255815133 ) ) ;
#11085 = CIRCLE ( 'NONE', #2725, 3.500000000000000888 ) ;
#11086 = DIRECTION ( 'NONE',  ( 0.000000000000000000, 0.000000000000000000, -1.000000000000000000 ) ) ;
#11087 = CARTESIAN_POINT ( 'NONE',  ( -5.452638258930639914, 3.000000000000000000, -13.97385902380748313 ) ) ;
#11088 = EDGE_CURVE ( 'NONE', #7728, #4686, #214, .T. ) ;
#11089 = ORIENTED_EDGE ( 'NONE', *, *, #8394, .F. ) ;
#11090 = CARTESIAN_POINT ( 'NONE',  ( 0.000000000000000000, 9.000000000000000000, 0.000000000000000000 ) ) ;
#11091 = ORIENTED_EDGE ( 'NONE', *, *, #7823, .T. ) ;
#11092 = ORIENTED_EDGE ( 'NONE', *, *, #8096, .T. ) ;
#11093 = DIRECTION ( 'NONE',  ( 0.000000000000000000, 1.000000000000000000, -0.000000000000000000 ) ) ;
#11094 = VERTEX_POINT ( 'NONE', #12812 ) ;
#11095 = AXIS2_PLACEMENT_3D ( 'NONE', #3679, #6855, #6931 ) ;
#11096 = CARTESIAN_POINT ( 'NONE',  ( -11.14709020439930676, 0.000000000000000000, -7.712570079660886257 ) ) ;
#11097 = AXIS2_PLACEMENT_3D ( 'NONE', #960, #12539, #1990 ) ;
#11098 = VERTEX_POINT ( 'NONE', #8665 ) ;
#11099 = CARTESIAN_POINT ( 'NONE',  ( 2.720000000000001528, 2.000000000000000000, 6.000000000000000000 ) ) ;
#11100 = PRESENTATION_STYLE_ASSIGNMENT (( #9225 ) ) ;
#11101 = DIRECTION ( 'NONE',  ( 0.000000000000000000, 0.000000000000000000, 1.000000000000000000 ) ) ;
#11102 = CARTESIAN_POINT ( 'NONE',  ( -6.970598036433426792, 3.000000000000000000, -10.97318381393771780 ) ) ;
#11103 = EDGE_CURVE ( 'NONE', #916, #4831, #12199, .T. ) ;
#11104 = CARTESIAN_POINT ( 'NONE',  ( -12.68816982652970893, 0.000000000000000000, 2.830255545554337004 ) ) ;
#11105 = CARTESIAN_POINT ( 'NONE',  ( 8.482622935103764306, 3.000000000000000000, -9.600126836553261711 ) ) ;
#11106 = CARTESIAN_POINT ( 'NONE',  ( -1.119409668803374558, 0.000000000000000000, -13.50845331674225669 ) ) ;
#11107 = ORIENTED_EDGE ( 'NONE', *, *, #4654, .T. ) ;
#11108 =( GEOMETRIC_REPRESENTATION_CONTEXT ( 3 ) GLOBAL_UNCERTAINTY_ASSIGNED_CONTEXT ( ( #8185 ) ) GLOBAL_UNIT_ASSIGNED_CONTEXT ( ( #1954, #6019, #8080 ) ) REPRESENTATION_CONTEXT ( 'NONE', 'WORKASPACE' ) );
#11109 = CARTESIAN_POINT ( 'NONE',  ( -13.73660796332618261, 3.000000000000000000, -6.025412986832017204 ) ) ;
#11110 = AXIS2_PLACEMENT_3D ( 'NONE', #13315, #3866, #4273 ) ;
#11111 = EDGE_LOOP ( 'NONE', ( #804, #38, #4854, #6592 ) ) ;
#11112 = ORIENTED_EDGE ( 'NONE', *, *, #6422, .T. ) ;
#11113 = CYLINDRICAL_SURFACE ( 'NONE', #4235, 12.08999999999737440 ) ;
#11114 = EDGE_LOOP ( 'NONE', ( #1034, #9175 ) ) ;
#11115 = FACE_OUTER_BOUND ( 'NONE', #1358, .T. ) ;
#11116 = AXIS2_PLACEMENT_3D ( 'NONE', #4878, #1660, #476 ) ;
#11117 = CARTESIAN_POINT ( 'NONE',  ( 8.922226997226882617, 3.000000000000000000, 8.158551673544282679 ) ) ;
#11118 = CARTESIAN_POINT ( 'NONE',  ( -8.914835885878284572, 3.000000000000000000, -11.11702303352191379 ) ) ;
#11119 = DIRECTION ( 'NONE',  ( 0.000000000000000000, 1.000000000000000000, 0.000000000000000000 ) ) ;
#11120 = EDGE_CURVE ( 'NONE', #4282, #843, #3597, .T. ) ;
#11121 = CARTESIAN_POINT ( 'NONE',  ( -4.190859029938718727, 9.000000000000000000, -6.054087828318142073 ) ) ;
#11122 = CARTESIAN_POINT ( 'NONE',  ( -5.170206418547117266, 3.000000000000000000, 13.27898586450088203 ) ) ;
#11123 = EDGE_CURVE ( 'NONE', #7795, #8354, #11309, .T. ) ;
#11124 = DIRECTION ( 'NONE',  ( -1.000000000000000000, -0.000000000000000000, -0.000000000000000000 ) ) ;
#11125 = DIRECTION ( 'NONE',  ( 0.000000000000000000, 0.000000000000000000, 1.000000000000000000 ) ) ;
#11126 = CARTESIAN_POINT ( 'NONE',  ( -14.08504230442586369, 0.000000000000000000, 2.161962830978781724 ) ) ;
#11127 = CARTESIAN_POINT ( 'NONE',  ( 5.571313494980132397, 3.000000000000000000, -10.72979803820131472 ) ) ;
#11128 = ORIENTED_EDGE ( 'NONE', *, *, #8948, .T. ) ;
#11129 = EDGE_LOOP ( 'NONE', ( #9862, #9889, #10955, #1181 ) ) ;
#11130 = VERTEX_POINT ( 'NONE', #9702 ) ;
#11131 = DIRECTION ( 'NONE',  ( -0.000000000000000000, -1.000000000000000000, -0.000000000000000000 ) ) ;
#11132 = CARTESIAN_POINT ( 'NONE',  ( -6.017756925049793537, 0.000000000000000000, -11.52330688609026232 ) ) ;
#11133 = EDGE_CURVE ( 'NONE', #7608, #8988, #7140, .T. ) ;
#11134 = ORIENTED_EDGE ( 'NONE', *, *, #5581, .F. ) ;
#11135 = DIRECTION ( 'NONE',  ( 0.4933917819034832619, -0.000000000000000000, -0.8698071910200015910 ) ) ;
#11136 = CARTESIAN_POINT ( 'NONE',  ( -13.28140389626389783, 3.000000000000000000, -1.567980996311402420 ) ) ;
#11137 = CARTESIAN_POINT ( 'NONE',  ( -11.11702303352197063, 0.000000000000000000, -8.914835885878215294 ) ) ;
#11138 = ADVANCED_FACE ( 'NONE', ( #11845 ), #2404, .F. ) ;
#11139 = FACE_OUTER_BOUND ( 'NONE', #12503, .T. ) ;
#11140 = EDGE_CURVE ( 'NONE', #7190, #3870, #6947, .T. ) ;
#11141 = CARTESIAN_POINT ( 'NONE',  ( 45.60964950616533287, 0.000000000000000000, -15.50984893380129392 ) ) ;
#11142 =( NAMED_UNIT ( * ) SI_UNIT ( $, .STERADIAN. ) SOLID_ANGLE_UNIT ( ) );
#11143 = ORIENTED_EDGE ( 'NONE', *, *, #8101, .T. ) ;
#11144 = ORIENTED_EDGE ( 'NONE', *, *, #12666, .F. ) ;
#11145 = VERTEX_POINT ( 'NONE', #619 ) ;
#11146 = CARTESIAN_POINT ( 'NONE',  ( 10.00000000000000533, 2.749999999999998224, -10.00000000000000178 ) ) ;
#11147 = EDGE_LOOP ( 'NONE', ( #6535, #12740, #13262, #1451 ) ) ;
#11148 = EDGE_CURVE ( 'NONE', #11016, #5839, #1349, .T. ) ;
#11149 = CARTESIAN_POINT ( 'NONE',  ( 10.72979803820131472, 0.000000000000000000, 5.571313494980131509 ) ) ;
#11150 = CARTESIAN_POINT ( 'NONE',  ( -2.047579527507185304, 35.33135765298362685, 9.239060114367257270 ) ) ;
#11151 = CARTESIAN_POINT ( 'NONE',  ( 1.557181465540758758, 3.000000000000000000, 14.16466328168009881 ) ) ;
#11152 = CYLINDRICAL_SURFACE ( 'NONE', #2213, 8.500000000000000000 ) ;
#11153 = LINE ( 'NONE', #9901, #6701 ) ;
#11154 = CARTESIAN_POINT ( 'NONE',  ( 0.000000000000000000, 3.000000000000000000, 0.000000000000000000 ) ) ;
#11155 = CARTESIAN_POINT ( 'NONE',  ( -13.00394681030572208, 3.000000000000000000, -0.1834665838397169235 ) ) ;
#11156 = ORIENTED_EDGE ( 'NONE', *, *, #3046, .F. ) ;
#11157 = CARTESIAN_POINT ( 'NONE',  ( -5.731782959214987372, 0.000000000000000000, -11.46814821560793618 ) ) ;
#11158 = ORIENTED_EDGE ( 'NONE', *, *, #8102, .T. ) ;
#11159 = ORIENTED_EDGE ( 'NONE', *, *, #12636, .F. ) ;
#11160 = DIRECTION ( 'NONE',  ( -0.000000000000000000, -1.000000000000000000, -0.000000000000000000 ) ) ;
#11161 = ORIENTED_EDGE ( 'NONE', *, *, #10779, .F. ) ;
#11162 = DIRECTION ( 'NONE',  ( 0.000000000000000000, 0.000000000000000000, 1.000000000000000000 ) ) ;
#11163 = EDGE_CURVE ( 'NONE', #5256, #1838, #10882, .T. ) ;
#11164 = ORIENTED_EDGE ( 'NONE', *, *, #2388, .T. ) ;
#11165 = FACE_OUTER_BOUND ( 'NONE', #4890, .T. ) ;
#11166 = SURFACE_STYLE_FILL_AREA ( #2895 ) ;
#11167 = CARTESIAN_POINT ( 'NONE',  ( 4.690415759823430619, 0.09999999999999982514, -1.500000000000000000 ) ) ;
#11168 = CARTESIAN_POINT ( 'NONE',  ( 9.133371500908369356, 3.000000000000000000, -11.90284147956862171 ) ) ;
#11169 = CARTESIAN_POINT ( 'NONE',  ( -2.830255545554292151, 0.000000000000000000, -12.68816982652971959 ) ) ;
#11170 = CARTESIAN_POINT ( 'NONE',  ( -6.506507307819711095, 3.000000000000000000, 10.18987059060247624 ) ) ;
#11171 = DIRECTION ( 'NONE',  ( -0.000000000000000000, -1.000000000000000000, -0.000000000000000000 ) ) ;
#11172 = ORIENTED_EDGE ( 'NONE', *, *, #7671, .F. ) ;
#11173 = CARTESIAN_POINT ( 'NONE',  ( 0.000000000000000000, 3.000000000000000000, 0.000000000000000000 ) ) ;
#11174 = ORIENTED_EDGE ( 'NONE', *, *, #12015, .T. ) ;
#11175 = B_SPLINE_CURVE_WITH_KNOTS ( 'NONE', 3,
 ( #9994, #10963, #495, #3793 ),
 .UNSPECIFIED., .F., .F.,
 ( 4, 4 ),
 ( 0.1547128134717859205, 1.000000000000000000 ),
 .UNSPECIFIED. ) ;
#11176 = ORIENTED_EDGE ( 'NONE', *, *, #1033, .F. ) ;
#11177 = CARTESIAN_POINT ( 'NONE',  ( 6.123233995736766282E-16, 3.000000000000000000, -5.000000000000000000 ) ) ;
#11178 = VERTEX_POINT ( 'NONE', #12055 ) ;
#11179 = DIRECTION ( 'NONE',  ( 0.000000000000000000, -0.000000000000000000, 1.000000000000000000 ) ) ;
#11180 = CARTESIAN_POINT ( 'NONE',  ( 31.00000000000000000, 3.000000000000000000, -3.499999999999999556 ) ) ;
#11181 = CARTESIAN_POINT ( 'NONE',  ( 5.985774866078160450, 0.000000000000000000, 3.119775513178307147 ) ) ;
#11182 = DIRECTION ( 'NONE',  ( -0.000000000000000000, -1.000000000000000000, -0.000000000000000000 ) ) ;
#11183 = B_SPLINE_CURVE_WITH_KNOTS ( 'NONE', 3,
 ( #7591, #1190, #3307, #8680 ),
 .UNSPECIFIED., .F., .F.,
 ( 4, 4 ),
 ( 0.000000000000000000, 0.5855695330273008592 ),
 .UNSPECIFIED. ) ;
#11184 = CARTESIAN_POINT ( 'NONE',  ( 3.893011711613070691, 3.000000000000000000, -12.40340517008307231 ) ) ;
#11185 = ITEM_DEFINED_TRANSFORMATION ( 'NONE', 'NONE', #1234,  #10007 ) ;
#11186 = CARTESIAN_POINT ( 'NONE',  ( 0.9098489087730803337, 9.000000000000000000, 7.307220250892556557 ) ) ;
#11187 = CARTESIAN_POINT ( 'NONE',  ( -9.375397774054503586, 0.000000000000000000, -11.70905276178452503 ) ) ;
#11188 = DIRECTION ( 'NONE',  ( 0.000000000000000000, -0.000000000000000000, -1.000000000000000000 ) ) ;
#11189 = CARTESIAN_POINT ( 'NONE',  ( 48.06174015963858892, 3.000000000000000000, -3.086958956539055166 ) ) ;
#11190 = DIRECTION ( 'NONE',  ( -0.000000000000000000, -1.000000000000000000, -0.000000000000000000 ) ) ;
#11191 =( REPRESENTATION_RELATIONSHIP ('NONE','NONE', #3798, #8461 ) REPRESENTATION_RELATIONSHIP_WITH_TRANSFORMATION ( #10428 )SHAPE_REPRESENTATION_RELATIONSHIP( ) );
#11192 = VERTEX_POINT ( 'NONE', #1448 ) ;
#11193 = EDGE_LOOP ( 'NONE', ( #1315, #3575, #2117, #2067 ) ) ;
#11194 = EDGE_CURVE ( 'NONE', #8041, #8258, #7774, .T. ) ;
#11195 = ORIENTED_EDGE ( 'NONE', *, *, #2133, .T. ) ;
#11196 = VERTEX_POINT ( 'NONE', #2605 ) ;
#11197 = CARTESIAN_POINT ( 'NONE',  ( -8.760376775873710997, 0.000000000000000000, 10.34346111134700941 ) ) ;
#11198 = CARTESIAN_POINT ( 'NONE',  ( 12.63269908545826503, 3.000000000000000000, -5.340493616518841691 ) ) ;
#11199 = CARTESIAN_POINT ( 'NONE',  ( -14.82803603298498629, 3.000000000000000000, 2.264806262023049577 ) ) ;
#11200 = CARTESIAN_POINT ( 'NONE',  ( 9.375397774054407662, 3.000000000000000000, -11.70905276178460497 ) ) ;
#11201 = FACE_OUTER_BOUND ( 'NONE', #10982, .T. ) ;
#11202 = CARTESIAN_POINT ( 'NONE',  ( 0.000000000000000000, 0.000000000000000000, -2.500000000000000444 ) ) ;
#11203 = CARTESIAN_POINT ( 'NONE',  ( 31.00000000000000000, 0.09999999999999982514, 0.000000000000000000 ) ) ;
#11204 = VERTEX_POINT ( 'NONE', #4751 ) ;
#11205 = ORIENTED_EDGE ( 'NONE', *, *, #3314, .F. ) ;
#11206 = EDGE_CURVE ( 'NONE', #11685, #4598, #11153, .T. ) ;
#11207 = ORIENTED_EDGE ( 'NONE', *, *, #10369, .F. ) ;
#11208 = DIRECTION ( 'NONE',  ( 0.000000000000000000, 0.000000000000000000, -1.000000000000000000 ) ) ;
#11209 = VERTEX_POINT ( 'NONE', #1723 ) ;
#11210 = EDGE_CURVE ( 'NONE', #6650, #1419, #8663, .T. ) ;
#11211 = EDGE_CURVE ( 'NONE', #912, #3761, #13348, .T. ) ;
#11212 = AXIS2_PLACEMENT_3D ( 'NONE', #13493, #7161, #11360 ) ;
#11213 = CARTESIAN_POINT ( 'NONE',  ( -8.430890348300632553, 0.000000000000000000, -11.48836750521723538 ) ) ;
#11214 = CARTESIAN_POINT ( 'NONE',  ( 15.17696780347026220, 44.33135765298363395, 35.00042399990225306 ) ) ;
#11215 = PLANE ( 'NONE',  #465 ) ;
#11216 = CARTESIAN_POINT ( 'NONE',  ( 11.63517940784358196, 3.000000000000000000, -7.494008246337187096 ) ) ;
#11217 = LINE ( 'NONE', #13565, #5160 ) ;
#11218 = CARTESIAN_POINT ( 'NONE',  ( -3.647470871583628593, 3.000000000000000000, 11.52666717836884125 ) ) ;
#11219 = CARTESIAN_POINT ( 'NONE',  ( -0.8123631076467130452, 9.000000000000000000, -6.700937709107178009 ) ) ;
#11220 = VERTEX_POINT ( 'NONE', #5848 ) ;
#11221 = CARTESIAN_POINT ( 'NONE',  ( -13.27898586450070084, 3.000000000000000000, -5.170206418547588001 ) ) ;
#11222 = AXIS2_PLACEMENT_3D ( 'NONE', #8144, #10290, #854 ) ;
#11223 = EDGE_CURVE ( 'NONE', #7786, #3089, #8724, .T. ) ;
#11224 = ORIENTED_EDGE ( 'NONE', *, *, #11243, .T. ) ;
#11225 = AXIS2_PLACEMENT_3D ( 'NONE', #647, #3732, #4447 ) ;
#11226 = ORIENTED_EDGE ( 'NONE', *, *, #6184, .F. ) ;
#11227 = DIRECTION ( 'NONE',  ( 0.6291930273682727615, 0.000000000000000000, -0.7772490812546181127 ) ) ;
#11228 = ORIENTED_EDGE ( 'NONE', *, *, #12735, .F. ) ;
#11229 = DIRECTION ( 'NONE',  ( 0.000000000000000000, 0.000000000000000000, -1.000000000000000000 ) ) ;
#11230 = EDGE_CURVE ( 'NONE', #9838, #1063, #2084, .T. ) ;
#11231 = VERTEX_POINT ( 'NONE', #6877 ) ;
#11232 = LINE ( 'NONE', #1804, #9146 ) ;
#11233 = SURFACE_STYLE_FILL_AREA ( #13376 ) ;
#11234 = VECTOR ( 'NONE', #5894, 1000.000000000000000 ) ;
#11235 = DIRECTION ( 'NONE',  ( 0.000000000000000000, 0.000000000000000000, 1.000000000000000000 ) ) ;
#11236 = DIRECTION ( 'NONE',  ( 0.7216024245882196597, 0.000000000000000000, -0.6923076923076926237 ) ) ;
#11237 = AXIS2_PLACEMENT_3D ( 'NONE', #5099, #9165, #6072 ) ;
#11238 = CARTESIAN_POINT ( 'NONE',  ( -13.50845331674225847, 0.000000000000000000, 1.119409668803372115 ) ) ;
#11239 = CARTESIAN_POINT ( 'NONE',  ( 0.7944557581062193785, 0.000000000000000000, -6.703084368289860429 ) ) ;
#11240 = DIRECTION ( 'NONE',  ( 0.000000000000000000, 1.000000000000000000, -0.000000000000000000 ) ) ;
#11241 = ORIENTED_EDGE ( 'NONE', *, *, #8756, .T. ) ;
#11242 = CARTESIAN_POINT ( 'NONE',  ( 0.000000000000000000, 0.000000000000000000, 0.000000000000000000 ) ) ;
#11243 = EDGE_CURVE ( 'NONE', #1347, #911, #2749, .T. ) ;
#11244 = ORIENTED_EDGE ( 'NONE', *, *, #770, .F. ) ;
#11245 = ADVANCED_FACE ( 'NONE', ( #3698, #8999, #3568 ), #13214, .F. ) ;
#11246 = ORIENTED_EDGE ( 'NONE', *, *, #12727, .T. ) ;
#11247 = FACE_OUTER_BOUND ( 'NONE', #4316, .T. ) ;
#11248 = VECTOR ( 'NONE', #12979, 1000.000000000000000 ) ;
#11249 = VECTOR ( 'NONE', #7558, 1000.000000000000000 ) ;
#11250 = VERTEX_POINT ( 'NONE', #5699 ) ;
#11251 = CARTESIAN_POINT ( 'NONE',  ( 5.250000000000000000, 3.000000000000000000, -27.94078293894052578 ) ) ;
#11252 = CARTESIAN_POINT ( 'NONE',  ( -13.33788847341978645, 3.000000000000000000, -2.414978278956336322 ) ) ;
#11253 = CARTESIAN_POINT ( 'NONE',  ( -8.504652361247167391, 0.000000000000000000, -9.593885948927674434 ) ) ;
#11254 = FACE_OUTER_BOUND ( 'NONE', #8244, .T. ) ;
#11255 = CARTESIAN_POINT ( 'NONE',  ( -0.4399887592034530392, 0.000000000000000000, 8.488604708182295511 ) ) ;
#11256 = CARTESIAN_POINT ( 'NONE',  ( 26.30958424017656938, 2.900000000000000355, 1.399999999999999911 ) ) ;
#11257 = VECTOR ( 'NONE', #5254, 1000.000000000000000 ) ;
#11258 = CARTESIAN_POINT ( 'NONE',  ( 1.836970198721030181E-16, 0.000000000000000000, 1.500000000000000222 ) ) ;
#11259 = LINE ( 'NONE', #7872, #9040 ) ;
#11260 = DIRECTION ( 'NONE',  ( 0.000000000000000000, 0.000000000000000000, -1.000000000000000000 ) ) ;
#11261 = CARTESIAN_POINT ( 'NONE',  ( -4.577511697546077230, 3.000000000000000000, -12.75843939030334795 ) ) ;
#11262 = VERTEX_POINT ( 'NONE', #7836 ) ;
#11263 = ORIENTED_EDGE ( 'NONE', *, *, #1229, .F. ) ;
#11264 = VERTEX_POINT ( 'NONE', #13087 ) ;
#11265 = CIRCLE ( 'NONE', #8398, 6.750000000000000888 ) ;
#11266 = ORIENTED_EDGE ( 'NONE', *, *, #8394, .T. ) ;
#11267 = CARTESIAN_POINT ( 'NONE',  ( 20.03271148078819408, 3.000000000000000000, -5.075121771833452478 ) ) ;
#11268 = DIRECTION ( 'NONE',  ( -1.000000000000000000, 3.491481338843133355E-15, 2.602085213965210149E-16 ) ) ;
#11269 = CARTESIAN_POINT ( 'NONE',  ( -14.90895795148409420, 3.000000000000000000, 1.650143266773909101 ) ) ;
#11270 =( REPRESENTATION_RELATIONSHIP ('NONE','NONE', #3798, #8461 ) REPRESENTATION_RELATIONSHIP_WITH_TRANSFORMATION ( #9038 )SHAPE_REPRESENTATION_RELATIONSHIP( ) );
#11271 = DIRECTION ( 'NONE',  ( 0.000000000000000000, 0.000000000000000000, 1.000000000000000000 ) ) ;
#11272 = DIRECTION ( 'NONE',  ( -0.000000000000000000, -1.000000000000000000, -0.000000000000000000 ) ) ;
#11273 = EDGE_CURVE ( 'NONE', #12695, #3555, #12862, .T. ) ;
#11274 = AXIS2_PLACEMENT_3D ( 'NONE', #4485, #8675, #2413 ) ;
#11275 = AXIS2_PLACEMENT_3D ( 'NONE', #1191, #2418, #6490 ) ;
#11276 = AXIS2_PLACEMENT_3D ( 'NONE', #4956, #10655, #3610 ) ;
#11277 = CARTESIAN_POINT ( 'NONE',  ( -12.07794044664754018, 0.000000000000000000, -0.5398653231797256868 ) ) ;
#11278 = CARTESIAN_POINT ( 'NONE',  ( 10.00000000000001776, 8.000000000000007105, -6.999999999999999112 ) ) ;
#11279 = ORIENTED_EDGE ( 'NONE', *, *, #5536, .T. ) ;
#11280 = CARTESIAN_POINT ( 'NONE',  ( 7.500000000000003553, 3.000000000000000000, 13.39999999999999858 ) ) ;
#11281 = CARTESIAN_POINT ( 'NONE',  ( 11.90284147956858085, 0.000000000000000000, -9.133371500908429752 ) ) ;
#11282 = VERTEX_POINT ( 'NONE', #11009 ) ;
#11283 = VECTOR ( 'NONE', #8723, 1000.000000000000000 ) ;
#11284 = AXIS2_PLACEMENT_3D ( 'NONE', #5829, #10029, #600 ) ;
#11285 = CIRCLE ( 'NONE', #7114, 14.25000000000000178 ) ;
#11286 = DIRECTION ( 'NONE',  ( -0.000000000000000000, -1.000000000000000000, -0.000000000000000000 ) ) ;
#11287 = CARTESIAN_POINT ( 'NONE',  ( 28.67696780347059970, 38.33135765298362685, 42.05042399990211521 ) ) ;
#11288 = EDGE_CURVE ( 'NONE', #11648, #12786, #9339, .T. ) ;
#11289 = CARTESIAN_POINT ( 'NONE',  ( 0.000000000000000000, 9.000000000000000000, 0.000000000000000000 ) ) ;
#11290 = CARTESIAN_POINT ( 'NONE',  ( 8.430890348300586368, 3.000000000000000000, -11.48836750521726913 ) ) ;
#11291 = EDGE_CURVE ( 'NONE', #11515, #5642, #474, .T. ) ;
#11292 = EDGE_CURVE ( 'NONE', #12227, #13024, #10258, .T. ) ;
#11293 = DIRECTION ( 'NONE',  ( -0.000000000000000000, -1.000000000000000000, -0.000000000000000000 ) ) ;
#11294 = DIRECTION ( 'NONE',  ( 0.000000000000000000, 1.000000000000000000, 0.000000000000000000 ) ) ;
#11295 = CARTESIAN_POINT ( 'NONE',  ( 3.000000000000001776, 2.000000000000000000, 7.000000000000000000 ) ) ;
#11296 = EDGE_LOOP ( 'NONE', ( #5059, #10340, #11741, #10041 ) ) ;
#11297 = VECTOR ( 'NONE', #9878, 1000.000000000000000 ) ;
#11298 = DIRECTION ( 'NONE',  ( 0.000000000000000000, 0.000000000000000000, -1.000000000000000000 ) ) ;
#11299 = AXIS2_PLACEMENT_3D ( 'NONE', #12449, #2025, #2921 ) ;
#11300 = EDGE_CURVE ( 'NONE', #10734, #12681, #8253, .T. ) ;
#11301 = CIRCLE ( 'NONE', #296, 6.750000000000000888 ) ;
#11302 = EDGE_LOOP ( 'NONE', ( #3223, #7095, #10706, #12293, #11771, #8271, #12110, #8002, #7767, #8505, #3785, #6465 ) ) ;
#11303 = EDGE_LOOP ( 'NONE', ( #6594, #2275, #9006, #11035 ) ) ;
#11304 = VERTEX_POINT ( 'NONE', #9213 ) ;
#11305 = CARTESIAN_POINT ( 'NONE',  ( 6.017756925049591921, 3.000000000000000000, -11.52330688609011844 ) ) ;
#11306 = ORIENTED_EDGE ( 'NONE', *, *, #2071, .T. ) ;
#11307 = DIRECTION ( 'NONE',  ( 0.000000000000000000, 1.000000000000000000, -0.000000000000000000 ) ) ;
#11308 = CIRCLE ( 'NONE', #6461, 3.000000000000000888 ) ;
#11309 = CIRCLE ( 'NONE', #5358, 6.750000000000000888 ) ;
#11310 = DIRECTION ( 'NONE',  ( 0.000000000000000000, 0.000000000000000000, 1.000000000000000000 ) ) ;
#11311 = EDGE_CURVE ( 'NONE', #10069, #3948, #9768, .T. ) ;
#11312 =( NAMED_UNIT ( * ) PLANE_ANGLE_UNIT ( ) SI_UNIT ( $, .RADIAN. ) );
#11313 = DIRECTION ( 'NONE',  ( 0.000000000000000000, 0.000000000000000000, 1.000000000000000000 ) ) ;
#11314 = LINE ( 'NONE', #11513, #10378 ) ;
#11315 = CARTESIAN_POINT ( 'NONE',  ( -11.46847481510586775, 3.000000000000000000, -5.708888906988912382 ) ) ;
#11316 = VERTEX_POINT ( 'NONE', #5017 ) ;
#11317 = EDGE_CURVE ( 'NONE', #5557, #8710, #8313, .T. ) ;
#11318 = LINE ( 'NONE', #845, #12831 ) ;
#11319 = ADVANCED_FACE ( 'NONE', ( #8377 ), #2956, .F. ) ;
#11320 = ORIENTED_EDGE ( 'NONE', *, *, #9388, .F. ) ;
#11321 = VERTEX_POINT ( 'NONE', #11425 ) ;
#11322 = AXIS2_PLACEMENT_3D ( 'NONE', #5685, #3756, #12933 ) ;
#11323 = CARTESIAN_POINT ( 'NONE',  ( -0.5398653231797316820, 3.000000000000000000, 12.07794044664754018 ) ) ;
#11324 = ORIENTED_EDGE ( 'NONE', *, *, #1854, .T. ) ;
#11325 = CARTESIAN_POINT ( 'NONE',  ( -1.604252589105048976, 9.000000000000000000, -8.347237484961699039 ) ) ;
#11326 = CARTESIAN_POINT ( 'NONE',  ( 11.70905276178455878, 3.000000000000000000, -9.375397774054460953 ) ) ;
#11327 = CARTESIAN_POINT ( 'NONE',  ( 4.652003457867571967, 9.000000000000000000, -6.437678087145717321 ) ) ;
#11328 = DIRECTION ( 'NONE',  ( 0.000000000000000000, 1.000000000000000000, 0.000000000000000000 ) ) ;
#11329 = EDGE_CURVE ( 'NONE', #12096, #13453, #8016, .T. ) ;
#11330 = CARTESIAN_POINT ( 'NONE',  ( 0.000000000000000000, 3.000000000000000000, 0.000000000000000000 ) ) ;
#11331 = VECTOR ( 'NONE', #4508, 1000.000000000000000 ) ;
#11332 = CARTESIAN_POINT ( 'NONE',  ( 1.557181465540758758, 3.000000000000000000, 14.16466328168009881 ) ) ;
#11333 = AXIS2_PLACEMENT_3D ( 'NONE', #10431, #2159, #5320 ) ;
#11334 = CARTESIAN_POINT ( 'NONE',  ( -5.250000000000000000, 0.000000000000000000, -27.94078293894052578 ) ) ;
#11335 = LINE ( 'NONE', #8218, #6852 ) ;
#11336 = CARTESIAN_POINT ( 'NONE',  ( 13.27898586450067420, 3.000000000000000000, 5.170206418547648397 ) ) ;
#11337 = FACE_OUTER_BOUND ( 'NONE', #9796, .T. ) ;
#11338 = VERTEX_POINT ( 'NONE', #3910 ) ;
#11339 = VERTEX_POINT ( 'NONE', #4181 ) ;
#11340 = VERTEX_POINT ( 'NONE', #13596 ) ;
#11341 = CIRCLE ( 'NONE', #5388, 0.1000000000000000472 ) ;
#11342 = ORIENTED_EDGE ( 'NONE', *, *, #6420, .F. ) ;
#11343 = LINE ( 'NONE', #8356, #13500 ) ;
#11344 = CARTESIAN_POINT ( 'NONE',  ( 0.000000000000000000, 0.000000000000000000, 0.000000000000000000 ) ) ;
#11345 = EDGE_CURVE ( 'NONE', #12325, #7402, #3837, .T. ) ;
#11346 = EDGE_CURVE ( 'NONE', #8207, #5642, #8229, .T. ) ;
#11347 = DIRECTION ( 'NONE',  ( 0.000000000000000000, 0.000000000000000000, -1.000000000000000000 ) ) ;
#11348 = CYLINDRICAL_SURFACE ( 'NONE', #7295, 12.08999999999737440 ) ;
#11349 = CARTESIAN_POINT ( 'NONE',  ( -0.8148820470561124463, 0.000000000000000000, 6.700631854488474204 ) ) ;
#11350 =( GEOMETRIC_REPRESENTATION_CONTEXT ( 3 ) GLOBAL_UNCERTAINTY_ASSIGNED_CONTEXT ( ( #4758 ) ) GLOBAL_UNIT_ASSIGNED_CONTEXT ( ( #13009, #348, #10941 ) ) REPRESENTATION_CONTEXT ( 'NONE', 'WORKASPACE' ) );
#11351 = CARTESIAN_POINT ( 'NONE',  ( 22.00000000000000000, 3.000000000000000000, 1.500000000000000666 ) ) ;
#11352 = CARTESIAN_POINT ( 'NONE',  ( -5.999999999999991118, 3.000000000000000000, 25.50000000000000000 ) ) ;
#11354 = VERTEX_POINT ( 'NONE', #5159 ) ;
#11353 = SHAPE_REPRESENTATION ( 'base-plate', ( #10007 ), #10678 ) ;
#11355 = CYLINDRICAL_SURFACE ( 'NONE', #2034, 1.500000000000001332 ) ;
#11356 = LINE ( 'NONE', #7351, #9077 ) ;
#11357 = B_SPLINE_CURVE_WITH_KNOTS ( 'NONE', 3,
 ( #5593, #10830, #6627, #3390 ),
 .UNSPECIFIED., .F., .F.,
 ( 4, 4 ),
 ( 0.1276832474596244493, 1.000000000000000000 ),
 .UNSPECIFIED. ) ;
#11358 = ORIENTED_EDGE ( 'NONE', *, *, #5636, .T. ) ;
#11359 = AXIS2_PLACEMENT_3D ( 'NONE', #3693, #7895, #7017 ) ;
#11360 = DIRECTION ( 'NONE',  ( 0.000000000000000000, 0.000000000000000000, -1.000000000000000000 ) ) ;
#11361 = APPLICATION_PROTOCOL_DEFINITION ( 'draft international standard', 'automotive_design', 1998, #5544 ) ;
#11362 = CARTESIAN_POINT ( 'NONE',  ( 1.105736515254441388, 0.000000000000000000, -13.50994833511691695 ) ) ;
#11363 = CARTESIAN_POINT ( 'NONE',  ( 11.48836750521724070, 3.000000000000000000, 8.430890348300627224 ) ) ;
#11364 = CARTESIAN_POINT ( 'NONE',  ( 30.80713437936438126, 0.000000000000000000, 0.9994049933487144655 ) ) ;
#11365 = CARTESIAN_POINT ( 'NONE',  ( 3.188443874008702661, 0.000000000000000000, -12.60833581801614578 ) ) ;
#11366 = B_SPLINE_SURFACE_WITH_KNOTS ( 'NONE', 3, 1, ( 
 ( #2321, #1341 ),
 ( #12722, #5469 ),
 ( #10585, #3471 ),
 ( #8501, #9676 ) ),
 .UNSPECIFIED., .F., .F., .F.,
 ( 4, 4 ),
 ( 2, 2 ),
 ( 0.000000000000000000, 0.8724294488011777871 ),
 ( 0.000000000000000000, 1.000000000000000000 ),
 .UNSPECIFIED. ) ;
#11367 = CARTESIAN_POINT ( 'NONE',  ( -12.51336114795298471, 0.000000000000000000, -3.542894103880322998 ) ) ;
#11368 = FACE_OUTER_BOUND ( 'NONE', #1003, .T. ) ;
#11369 = ORIENTED_EDGE ( 'NONE', *, *, #1359, .T. ) ;
#11370 = EDGE_LOOP ( 'NONE', ( #9906, #8814, #12848, #2753 ) ) ;
#11371 = CARTESIAN_POINT ( 'NONE',  ( 1.836970198721030181E-16, 3.000000000000000000, 1.500000000000000222 ) ) ;
#11372 = EDGE_CURVE ( 'NONE', #1409, #1736, #7362, .T. ) ;
#11373 = ORIENTED_EDGE ( 'NONE', *, *, #2072, .F. ) ;
#11374 = CARTESIAN_POINT ( 'NONE',  ( 2.392396671352951198, 9.000000000000000000, 6.311809420990095454 ) ) ;
#11375 = DIRECTION ( 'NONE',  ( -0.000000000000000000, -1.000000000000000000, 0.000000000000000000 ) ) ;
#11376 = CARTESIAN_POINT ( 'NONE',  ( 8.093005444143644311, 9.000000000000000000, -2.598704077239528232 ) ) ;
#11377 = CARTESIAN_POINT ( 'NONE',  ( -12.40347894490204972, 3.000000000000000000, 3.892776652129660064 ) ) ;
#11378 = DIRECTION ( 'NONE',  ( 0.000000000000000000, 0.000000000000000000, -1.000000000000000000 ) ) ;
#11379 = ORIENTED_EDGE ( 'NONE', *, *, #7702, .F. ) ;
#11380 = CARTESIAN_POINT ( 'NONE',  ( 26.30958424017656938, 3.000000000000000000, -4.500000000000000888 ) ) ;
#11381 = EDGE_LOOP ( 'NONE', ( #10519, #7801, #2162, #10704 ) ) ;
#11382 = ORIENTED_EDGE ( 'NONE', *, *, #4930, .F. ) ;
#11383 = CARTESIAN_POINT ( 'NONE',  ( -11.52666717836884125, 3.000000000000000000, -3.647470871583627705 ) ) ;
#11384 = EDGE_CURVE ( 'NONE', #10060, #3498, #11217, .T. ) ;
#11385 = B_SPLINE_CURVE_WITH_KNOTS ( 'NONE', 3,
 ( #4792, #6854, #1764, #8978 ),
 .UNSPECIFIED., .F., .F.,
 ( 4, 4 ),
 ( 0.000000000000000000, 0.8452273900860258760 ),
 .UNSPECIFIED. ) ;
#11386 = ADVANCED_FACE ( 'NONE', ( #12482 ), #387, .F. ) ;
#11387 = ORIENTED_EDGE ( 'NONE', *, *, #6021, .T. ) ;
#11388 = EDGE_CURVE ( 'NONE', #10891, #5504, #8231, .T. ) ;
#11389 = FACE_OUTER_BOUND ( 'NONE', #4740, .T. ) ;
#11390 = EDGE_CURVE ( 'NONE', #5917, #13298, #5110, .T. ) ;
#11391 = CARTESIAN_POINT ( 'NONE',  ( 4.690415759823430619, 0.1000000000000000056, -1.500000000000000000 ) ) ;
#11392 = EDGE_CURVE ( 'NONE', #12695, #8040, #6916, .T. ) ;
#11393 = CARTESIAN_POINT ( 'NONE',  ( 3.647599401157688437, 0.000000000000000000, 11.52662650599083882 ) ) ;
#11394 = DIRECTION ( 'NONE',  ( -0.000000000000000000, -1.000000000000000000, -0.000000000000000000 ) ) ;
#11395 = CARTESIAN_POINT ( 'NONE',  ( -10.15083332828461771, 3.000000000000000000, -29.86148447151320795 ) ) ;
#11396 = CARTESIAN_POINT ( 'NONE',  ( 11.70905276178455878, 3.000000000000000000, -9.375397774054460953 ) ) ;
#11397 = CARTESIAN_POINT ( 'NONE',  ( 2.392396671352951198, 0.000000000000000000, 6.311809420990095454 ) ) ;
#11398 = CARTESIAN_POINT ( 'NONE',  ( 45.22938609343211880, 0.000000000000000000, -15.43472716196784233 ) ) ;
#11399 = LINE ( 'NONE', #1961, #12450 ) ;
#11400 = ORIENTED_EDGE ( 'NONE', *, *, #92, .T. ) ;
#11401 = LINE ( 'NONE', #9331, #3792 ) ;
#11402 = VERTEX_POINT ( 'NONE', #4119 ) ;
#11403 = EDGE_LOOP ( 'NONE', ( #9961, #1326, #7888, #6515 ) ) ;
#11404 = EDGE_CURVE ( 'NONE', #5785, #9584, #327, .T. ) ;
#11405 = VERTEX_POINT ( 'NONE', #1026 ) ;
#11406 = ORIENTED_EDGE ( 'NONE', *, *, #3216, .F. ) ;
#11407 = DIRECTION ( 'NONE',  ( 0.000000000000000000, 0.000000000000000000, 1.000000000000000000 ) ) ;
#11408 = DIRECTION ( 'NONE',  ( 0.000000000000000000, 0.000000000000000000, 1.000000000000000000 ) ) ;
#11409 = EDGE_CURVE ( 'NONE', #7235, #10517, #12337, .T. ) ;
#11410 = CARTESIAN_POINT ( 'NONE',  ( -3.833392836528144443, 9.000000000000000000, -5.555861711818853799 ) ) ;
#11411 = DIRECTION ( 'NONE',  ( 0.6291930273683257191, 0.000000000000000000, -0.7772490812545752581 ) ) ;
#11412 = DIRECTION ( 'NONE',  ( 0.000000000000000000, 0.000000000000000000, 1.000000000000000000 ) ) ;
#11413 = FACE_OUTER_BOUND ( 'NONE', #5423, .T. ) ;
#11414 = DIRECTION ( 'NONE',  ( 0.000000000000000000, 0.000000000000000000, 1.000000000000000000 ) ) ;
#11415 = EDGE_LOOP ( 'NONE', ( #2316, #2051, #12957, #5376 ) ) ;
#11416 = CARTESIAN_POINT ( 'NONE',  ( 0.000000000000000000, 3.000000000000000000, 0.000000000000000000 ) ) ;
#11417 = EDGE_CURVE ( 'NONE', #3822, #9443, #6933, .T. ) ;
#11418 = CARTESIAN_POINT ( 'NONE',  ( -18.21140389626389222, 3.000000000000000000, 12.49772878833446299 ) ) ;
#11419 = B_SPLINE_SURFACE_WITH_KNOTS ( 'NONE', 2, 1, ( 
 ( #2376, #3331 ),
 ( #8761, #2235 ),
 ( #11751, #9670 ) ),
 .UNSPECIFIED., .F., .F., .F.,
 ( 3, 3 ),
 ( 2, 2 ),
 ( 0.000000000000000000, 1.000000000000000000 ),
 ( 0.000000000000000000, 1.000000000000000000 ),
 .UNSPECIFIED. ) ;
#11420 = VERTEX_POINT ( 'NONE', #10729 ) ;
#11421 = DIRECTION ( 'NONE',  ( 0.000000000000000000, 0.000000000000000000, -1.000000000000000000 ) ) ;
#11422 = SHAPE_DEFINITION_REPRESENTATION ( #4246, #6537 ) ;
#11423 = DIRECTION ( 'NONE',  ( 0.000000000000000000, 1.000000000000000000, 0.000000000000000000 ) ) ;
#11424 = CARTESIAN_POINT ( 'NONE',  ( 0.000000000000000000, 13.00000000000000178, 0.000000000000000000 ) ) ;
#11425 = CARTESIAN_POINT ( 'NONE',  ( 2.604399508763944660, 0.000000000000000000, -11.80615107470197600 ) ) ;
#11426 = CARTESIAN_POINT ( 'NONE',  ( -12.60833596047604210, 3.000000000000000000, -3.188441730140805674 ) ) ;
#11427 = CARTESIAN_POINT ( 'NONE',  ( -13.97385902380755240, 3.000000000000000000, -5.452638258930474713 ) ) ;
#11428 = EDGE_LOOP ( 'NONE', ( #11852, #10749, #6100, #5932 ) ) ;
#11429 = ORIENTED_EDGE ( 'NONE', *, *, #13521, .F. ) ;
#11430 = CARTESIAN_POINT ( 'NONE',  ( 4.690415759823430619, 3.000000000000000000, -4.500000000000000888 ) ) ;
#11431 = VECTOR ( 'NONE', #12536, 1000.000000000000000 ) ;
#11432 = VERTEX_POINT ( 'NONE', #11831 ) ;
#11433 = CARTESIAN_POINT ( 'NONE',  ( 2.719999999999997087, 0.000000000000000000, -6.000000000000000000 ) ) ;
#11434 = DIRECTION ( 'NONE',  ( 0.000000000000000000, 0.000000000000000000, -1.000000000000000000 ) ) ;
#11435 = CARTESIAN_POINT ( 'NONE',  ( 28.54655175640005282, 0.09999999999999982514, 2.353846153846154809 ) ) ;
#11436 = CARTESIAN_POINT ( 'NONE',  ( 0.5501230721522984979, 3.000000000000000000, -12.98835496148321766 ) ) ;
#11437 = AXIS2_PLACEMENT_3D ( 'NONE', #8233, #6045, #1844 ) ;
#11438 = DIRECTION ( 'NONE',  ( 0.000000000000000000, 0.000000000000000000, 1.000000000000000000 ) ) ;
#11439 = CIRCLE ( 'NONE', #6161, 6.750000000000000888 ) ;
#11440 = DIRECTION ( 'NONE',  ( -0.000000000000000000, -1.000000000000000000, -0.000000000000000000 ) ) ;
#11441 = EDGE_CURVE ( 'NONE', #7238, #9762, #4252, .T. ) ;
#11442 = ORIENTED_EDGE ( 'NONE', *, *, #10938, .F. ) ;
#11443 = DIRECTION ( 'NONE',  ( 0.000000000000000000, 0.000000000000000000, 1.000000000000000000 ) ) ;
#11444 = ORIENTED_EDGE ( 'NONE', *, *, #4337, .F. ) ;
#11445 = ORIENTED_EDGE ( 'NONE', *, *, #11163, .T. ) ;
#11446 = DIRECTION ( 'NONE',  ( 0.000000000000000000, 0.000000000000000000, -1.000000000000000000 ) ) ;
#11447 = ORIENTED_EDGE ( 'NONE', *, *, #9107, .T. ) ;
#11448 = AXIS2_PLACEMENT_3D ( 'NONE', #7524, #7835, #12764 ) ;
#11449 = CIRCLE ( 'NONE', #2429, 14.25000000000000355 ) ;
#11450 = DIRECTION ( 'NONE',  ( 0.000000000000000000, 0.000000000000000000, 1.000000000000000000 ) ) ;
#11451 = CARTESIAN_POINT ( 'NONE',  ( 41.29994854050690378, 3.000000000000000000, -5.141175130212632283 ) ) ;
#11452 = CARTESIAN_POINT ( 'NONE',  ( -5.731782959214987372, 0.000000000000000000, -11.46814821560793618 ) ) ;
#11453 = CARTESIAN_POINT ( 'NONE',  ( 13.50000000000000355, 3.000000000000000000, -7.050000000000000711 ) ) ;
#11454 = CARTESIAN_POINT ( 'NONE',  ( 23.99887587215152607, 0.000000000000000000, 4.000000000000000000 ) ) ;
#11455 = ITEM_DEFINED_TRANSFORMATION ( 'NONE', 'NONE', #3423,  #10007 ) ;
#11456 = CARTESIAN_POINT ( 'NONE',  ( 13.50000000000000355, 3.000000000000000000, -7.050000000000000711 ) ) ;
#11457 = CARTESIAN_POINT ( 'NONE',  ( -4.334442004268525217, 9.000000000000000000, 7.311813216407587745 ) ) ;
#11458 = DIRECTION ( 'NONE',  ( 0.000000000000000000, 1.000000000000000000, 0.000000000000000000 ) ) ;
#11459 = EDGE_CURVE ( 'NONE', #3932, #9838, #2639, .T. ) ;
#11460 = ORIENTED_EDGE ( 'NONE', *, *, #2322, .F. ) ;
#11461 = CARTESIAN_POINT ( 'NONE',  ( 0.000000000000000000, 9.000000000000000000, 0.000000000000000000 ) ) ;
#11462 = CIRCLE ( 'NONE', #9029, 12.08999999999737263 ) ;
#11463 = AXIS2_PLACEMENT_3D ( 'NONE', #8311, #4383, #3079 ) ;
#11464 = EDGE_LOOP ( 'NONE', ( #2189, #3966, #11324, #4700 ) ) ;
#11465 = ORIENTED_EDGE ( 'NONE', *, *, #1964, .T. ) ;
#11466 = EDGE_CURVE ( 'NONE', #11838, #5374, #11546, .T. ) ;
#11467 = ORIENTED_EDGE ( 'NONE', *, *, #11292, .F. ) ;
#11468 = ORIENTED_EDGE ( 'NONE', *, *, #7913, .F. ) ;
#11469 = CARTESIAN_POINT ( 'NONE',  ( -8.100301009650799244, 0.000000000000000000, -2.575873357339268033 ) ) ;
#11470 = B_SPLINE_CURVE_WITH_KNOTS ( 'NONE', 3,
 ( #11990, #2473, #3567, #757 ),
 .UNSPECIFIED., .F., .F.,
 ( 4, 4 ),
 ( 0.000000000000000000, 0.5855695330273008592 ),
 .UNSPECIFIED. ) ;
#11471 = DIRECTION ( 'NONE',  ( 0.000000000000000000, 0.000000000000000000, 1.000000000000000000 ) ) ;
#11472 = VECTOR ( 'NONE', #3671, 1000.000000000000114 ) ;
#11473 = CIRCLE ( 'NONE', #3283, 4.000000000000000000 ) ;
#11474 = DIRECTION ( 'NONE',  ( 0.000000000000000000, 0.000000000000000000, 1.000000000000000000 ) ) ;
#11475 = EDGE_CURVE ( 'NONE', #7781, #11595, #9756, .T. ) ;
#11476 = CARTESIAN_POINT ( 'NONE',  ( 0.5398653231797245766, 3.000000000000000000, -12.07794044664754018 ) ) ;
#11477 = CARTESIAN_POINT ( 'NONE',  ( 1.557181465540758758, 3.000000000000000000, 14.16466328168009881 ) ) ;
#11478 = ORIENTED_EDGE ( 'NONE', *, *, #198, .T. ) ;
#11479 = EDGE_CURVE ( 'NONE', #732, #447, #3178, .T. ) ;
#11480 = AXIS2_PLACEMENT_3D ( 'NONE', #10701, #9657, #9596 ) ;
#11481 = DIRECTION ( 'NONE',  ( 0.000000000000000000, 0.000000000000000000, -1.000000000000000000 ) ) ;
#11482 = CARTESIAN_POINT ( 'NONE',  ( 13.04554897075799502, 0.000000000000000000, 5.733772933379473358 ) ) ;
#11483 = ORIENTED_EDGE ( 'NONE', *, *, #7416, .T. ) ;
#11484 = CARTESIAN_POINT ( 'NONE',  ( 28.47439151394123158, 3.000000000000000000, 2.423076923076924238 ) ) ;
#11485 = CARTESIAN_POINT ( 'NONE',  ( 26.30958424017656938, 0.000000000000000000, -1.399999999999999911 ) ) ;
#11486 = AXIS2_PLACEMENT_3D ( 'NONE', #9744, #7680, #7417 ) ;
#11487 = SHAPE_DEFINITION_REPRESENTATION ( #13146, #7939 ) ;
#11488 = CIRCLE ( 'NONE', #5755, 1.000000000000000888 ) ;
#11489 = EDGE_CURVE ( 'NONE', #3238, #10765, #2297, .T. ) ;
#11490 = CARTESIAN_POINT ( 'NONE',  ( 49.72134184781355515, 3.000000000000000000, -3.261665100124877981 ) ) ;
#11491 = CARTESIAN_POINT ( 'NONE',  ( 5.170206418547604876, 0.000000000000000000, -13.27898586450069196 ) ) ;
#11492 = EDGE_CURVE ( 'NONE', #10414, #11737, #4386, .T. ) ;
#11493 = DIRECTION ( 'NONE',  ( -0.000000000000000000, -1.000000000000000000, -0.000000000000000000 ) ) ;
#11494 = CARTESIAN_POINT ( 'NONE',  ( -14.20034848914876235, 0.000000000000000000, -2.631756770590732764 ) ) ;
#11495 = CARTESIAN_POINT ( 'NONE',  ( -11.11702303352197063, 0.000000000000000000, -8.914835885878215294 ) ) ;
#11496 = ADVANCED_FACE ( 'NONE', ( #3149, #142 ), #7361, .F. ) ;
#11497 = ORIENTED_EDGE ( 'NONE', *, *, #197, .T. ) ;
#11498 = VECTOR ( 'NONE', #3988, 1000.000000000000000 ) ;
#11499 = ORIENTED_EDGE ( 'NONE', *, *, #5965, .T. ) ;
#11500 = DIRECTION ( 'NONE',  ( 2.602085213965207190E-16, -8.673617379884034239E-17, 1.000000000000000000 ) ) ;
#11501 = AXIS2_PLACEMENT_3D ( 'NONE', #3939, #10348, #13460 ) ;
#11502 = VECTOR ( 'NONE', #8616, 1000.000000000000000 ) ;
#11503 = EDGE_LOOP ( 'NONE', ( #10507, #11478, #1425, #7118 ) ) ;
#11504 = DIRECTION ( 'NONE',  ( 0.000000000000000000, 0.000000000000000000, 1.000000000000000000 ) ) ;
#11505 =( NAMED_UNIT ( * ) PLANE_ANGLE_UNIT ( ) SI_UNIT ( $, .RADIAN. ) );
#11506 = CARTESIAN_POINT ( 'NONE',  ( -8.430890348300124515, 0.000000000000000000, 11.48836750521761019 ) ) ;
#11507 = DIRECTION ( 'NONE',  ( 0.000000000000000000, 0.000000000000000000, -1.000000000000000000 ) ) ;
#11508 = EDGE_CURVE ( 'NONE', #1584, #6704, #4942, .T. ) ;
#11509 = CIRCLE ( 'NONE', #952, 8.499999999999996447 ) ;
#11510 = CARTESIAN_POINT ( 'NONE',  ( -3.893011711613112880, 0.000000000000000000, -12.40340517008282717 ) ) ;
#11511 = AXIS2_PLACEMENT_3D ( 'NONE', #9341, #7473, #11474 ) ;
#11512=STYLED_ITEM('',(#13642),#8440);
#11513 = CARTESIAN_POINT ( 'NONE',  ( 6.506620931068707314, 3.000000000000000000, 10.18979803820051622 ) ) ;
#11514 = CARTESIAN_POINT ( 'NONE',  ( -11.46847481510586775, 0.000000000000000000, -5.708888906988912382 ) ) ;
#11515 = VERTEX_POINT ( 'NONE', #6381 ) ;
#11516 = CARTESIAN_POINT ( 'NONE',  ( 30.80713437936438126, 3.000000000000000000, 0.9994049933487144655 ) ) ;
#11517 = VERTEX_POINT ( 'NONE', #10788 ) ;
#11518 = ORIENTED_EDGE ( 'NONE', *, *, #987, .T. ) ;
#11519 = LINE ( 'NONE', #6750, #7740 ) ;
#11521 = VERTEX_POINT ( 'NONE', #11572 ) ;
#11520 = B_SPLINE_CURVE_WITH_KNOTS ( 'NONE', 3,
 ( #7957, #10991, #1769, #11066 ),
 .UNSPECIFIED., .F., .F.,
 ( 4, 4 ),
 ( 0.8181806201944104018, 0.8475986972523573693 ),
 .UNSPECIFIED. ) ;
#11522 = VECTOR ( 'NONE', #9817, 1000.000000000000000 ) ;
#11523 = VECTOR ( 'NONE', #8344, 1000.000000000000000 ) ;
#11524 = AXIS2_PLACEMENT_3D ( 'NONE', #7366, #1231, #12801 ) ;
#11525 = CARTESIAN_POINT ( 'NONE',  ( -9.299128225235689271, 3.000000000000000000, -10.25006213149501555 ) ) ;
#11526 = CARTESIAN_POINT ( 'NONE',  ( 0.5398653231797245766, 3.000000000000000000, -12.07794044664754018 ) ) ;
#11527 = CARTESIAN_POINT ( 'NONE',  ( 1.650143266773734796, 3.000000000000000000, -14.90895795148410841 ) ) ;
#11528 = CARTESIAN_POINT ( 'NONE',  ( -5.784789447945489549, 3.000000000000000000, 12.25836857253663581 ) ) ;
#11529 = CARTESIAN_POINT ( 'NONE',  ( -7.125870497355421662, 0.000000000000000000, -3.507536778237742237 ) ) ;
#11530 = CARTESIAN_POINT ( 'NONE',  ( 11.63517940784358196, 0.000000000000000000, -7.494008246337187096 ) ) ;
#11531 = B_SPLINE_CURVE_WITH_KNOTS ( 'NONE', 3,
 ( #10894, #13101, #5786, #2560 ),
 .UNSPECIFIED., .F., .F.,
 ( 4, 4 ),
 ( 0.000000000000000000, 0.8724294488011757887 ),
 .UNSPECIFIED. ) ;
#11532 = DIRECTION ( 'NONE',  ( -1.000000000000000000, 0.000000000000000000, -0.000000000000000000 ) ) ;
#11533 = ORIENTED_EDGE ( 'NONE', *, *, #8254, .T. ) ;
#11534 = AXIS2_PLACEMENT_3D ( 'NONE', #10987, #1559, #9879 ) ;
#11535 = CARTESIAN_POINT ( 'NONE',  ( -6.549210654805285081, 9.000000000000000000, 1.634117437329677180 ) ) ;
#11536 = CIRCLE ( 'NONE', #4703, 0.7499999999999997780 ) ;
#11537 = VERTEX_POINT ( 'NONE', #5553 ) ;
#11538 = B_SPLINE_CURVE_WITH_KNOTS ( 'NONE', 3,
 ( #11932, #10635, #12765, #2495 ),
 .UNSPECIFIED., .F., .F.,
 ( 4, 4 ),
 ( 0.000000000000000000, 0.5855695330273008592 ),
 .UNSPECIFIED. ) ;
#11539 = ORIENTED_EDGE ( 'NONE', *, *, #3657, .F. ) ;
#11540 = ORIENTED_EDGE ( 'NONE', *, *, #9769, .T. ) ;
#11541 = EDGE_CURVE ( 'NONE', #2998, #6481, #7560, .T. ) ;
#11542 = ORIENTED_EDGE ( 'NONE', *, *, #9513, .T. ) ;
#11543 = DIRECTION ( 'NONE',  ( -0.000000000000000000, -1.000000000000000000, -0.000000000000000000 ) ) ;
#11545 = EDGE_CURVE ( 'NONE', #933, #11943, #10528, .T. ) ;
#11544 = VECTOR ( 'NONE', #1136, 1000.000000000000000 ) ;
#11547 = EDGE_CURVE ( 'NONE', #10838, #1061, #7787, .T. ) ;
#11546 = CIRCLE ( 'NONE', #11974, 1.500000000000000666 ) ;
#11548 = CARTESIAN_POINT ( 'NONE',  ( 28.47439151394123158, 0.09999999999999982514, 2.423076923076924238 ) ) ;
#11549 = AXIS2_PLACEMENT_3D ( 'NONE', #2087, #6348, #10493 ) ;
#11550 = DIRECTION ( 'NONE',  ( -0.000000000000000000, -1.000000000000000000, -0.000000000000000000 ) ) ;
#11551 = DIRECTION ( 'NONE',  ( 0.000000000000000000, 0.000000000000000000, -1.000000000000000000 ) ) ;
#11552 = DIRECTION ( 'NONE',  ( 0.000000000000000000, 0.000000000000000000, -1.000000000000000000 ) ) ;
#11553 = B_SPLINE_CURVE_WITH_KNOTS ( 'NONE', 3,
 ( #10497, #9394, #798, #5118 ),
 .UNSPECIFIED., .F., .F.,
 ( 4, 4 ),
 ( 0.1547128134717859205, 1.000000000000000000 ),
 .UNSPECIFIED. ) ;
#11554 = ORIENTED_EDGE ( 'NONE', *, *, #346, .T. ) ;
#11555 = AXIS2_PLACEMENT_3D ( 'NONE', #2106, #7610, #3203 ) ;
#11556 = VECTOR ( 'NONE', #10760, 1000.000000000000000 ) ;
#11557 = ORIENTED_EDGE ( 'NONE', *, *, #1066, .F. ) ;
#11558 = CARTESIAN_POINT ( 'NONE',  ( 31.00000000000000000, 0.000000000000000000, -4.000000001073670930 ) ) ;
#11559 = CARTESIAN_POINT ( 'NONE',  ( 4.355042381134426321, 9.000000000000000000, 7.299562031966228659 ) ) ;
#11560 = ADVANCED_FACE ( 'NONE', ( #8512 ), #4219, .F. ) ;
#11561 = EDGE_CURVE ( 'NONE', #2665, #10780, #10228, .T. ) ;
#11562 = ORIENTED_EDGE ( 'NONE', *, *, #1343, .T. ) ;
#11563 = CARTESIAN_POINT ( 'NONE',  ( 3.850308450823737516, 9.000000000000000000, 5.544152309732777617 ) ) ;
#11564 = FACE_OUTER_BOUND ( 'NONE', #946, .T. ) ;
#11565 = CIRCLE ( 'NONE', #4734, 1.500000000000001332 ) ;
#11566 = EDGE_CURVE ( 'NONE', #1266, #11231, #12672, .T. ) ;
#11567 = APPLICATION_PROTOCOL_DEFINITION ( 'draft international standard', 'automotive_design', 1998, #10569 ) ;
#11568 = CIRCLE ( 'NONE', #7813, 1.499999999999997780 ) ;
#11569 = ADVANCED_FACE ( 'NONE', ( #10033 ), #2592, .T. ) ;
#11570 = CARTESIAN_POINT ( 'NONE',  ( 51.41686768994642165, 0.000000000000000000, -11.86457109001525545 ) ) ;
#11571 = CARTESIAN_POINT ( 'NONE',  ( 3.647470871583629926, 0.000000000000000000, -11.52666717836884125 ) ) ;
#11572 = CARTESIAN_POINT ( 'NONE',  ( 28.54655175640005282, 3.000000000000000000, 2.353846153846155254 ) ) ;
#11573 = CARTESIAN_POINT ( 'NONE',  ( 41.29994854050690378, 3.000000000000000000, -6.141175130212632283 ) ) ;
#11574 = CARTESIAN_POINT ( 'NONE',  ( 5.452638258930520010, 3.000000000000000000, -13.97385902380752754 ) ) ;
#11575 = ORIENTED_EDGE ( 'NONE', *, *, #2045, .T. ) ;
#11576 = ORIENTED_EDGE ( 'NONE', *, *, #13410, .F. ) ;
#11577 = VERTEX_POINT ( 'NONE', #6859 ) ;
#11578 = LINE ( 'NONE', #2131, #2701 ) ;
#11579 = EDGE_CURVE ( 'NONE', #3916, #12227, #5130, .T. ) ;
#11580 = EDGE_LOOP ( 'NONE', ( #5743, #13164, #2817, #3998 ) ) ;
#11581 = CARTESIAN_POINT ( 'NONE',  ( -5.977417671213807182, 9.000000000000000000, 3.135757960025121527 ) ) ;
#11582 = CARTESIAN_POINT ( 'NONE',  ( -13.27898586450066709, 0.000000000000000000, 5.170206418547661720 ) ) ;
#11583 = CARTESIAN_POINT ( 'NONE',  ( -11.11702303352197063, 3.000000000000000000, -8.914835885878215294 ) ) ;
#11584 = CARTESIAN_POINT ( 'NONE',  ( 1.133238802859644956, 0.000000000000000000, -14.39763212228013600 ) ) ;
#11585 = DIRECTION ( 'NONE',  ( -0.000000000000000000, -1.000000000000000000, -0.000000000000000000 ) ) ;
#11586 = DIRECTION ( 'NONE',  ( 0.000000000000000000, 1.000000000000000000, 0.000000000000000000 ) ) ;
#11587 = VERTEX_POINT ( 'NONE', #7961 ) ;
#11588 = DIRECTION ( 'NONE',  ( -0.000000000000000000, -1.000000000000000000, -0.000000000000000000 ) ) ;
#11589 = VERTEX_POINT ( 'NONE', #4797 ) ;
#11590 = ORIENTED_EDGE ( 'NONE', *, *, #4376, .F. ) ;
#11591 = ORIENTED_EDGE ( 'NONE', *, *, #7611, .T. ) ;
#11592 = LINE ( 'NONE', #10622, #10395 ) ;
#11593 = ADVANCED_FACE ( 'NONE', ( #3482 ), #10094, .T. ) ;
#11594 = EDGE_CURVE ( 'NONE', #2964, #5704, #457, .T. ) ;
#11595 = VERTEX_POINT ( 'NONE', #6787 ) ;
#11596 = FACE_OUTER_BOUND ( 'NONE', #7451, .T. ) ;
#11597 = CARTESIAN_POINT ( 'NONE',  ( 9.065480927540312095, 0.000000000000000000, -9.324856600128422102 ) ) ;
#11598 = CARTESIAN_POINT ( 'NONE',  ( 46.02418392430381999, 0.000000000000000000, -15.41988256844266658 ) ) ;
#11599 = DIRECTION ( 'NONE',  ( -0.000000000000000000, -1.000000000000000000, -0.000000000000000000 ) ) ;
#11600 = CARTESIAN_POINT ( 'NONE',  ( -2.546103534247749600, 3.000000000000000000, 12.55526518755974585 ) ) ;
#11601 = LINE ( 'NONE', #9526, #519 ) ;
#11602 = CARTESIAN_POINT ( 'NONE',  ( 10.14701493152832512, 3.000000000000000000, -29.73855628788322747 ) ) ;
#11603 = CARTESIAN_POINT ( 'NONE',  ( 31.00000000000000000, 3.000000000000000000, -4.000000001073670930 ) ) ;
#11604 = ORIENTED_EDGE ( 'NONE', *, *, #6588, .F. ) ;
#11605 = CARTESIAN_POINT ( 'NONE',  ( 11.46814821560793618, 3.000000000000000000, -5.731782959214992701 ) ) ;
#11606 = B_SPLINE_SURFACE_WITH_KNOTS ( 'NONE', 3, 1, ( 
 ( #10582, #6304 ),
 ( #55, #1789 ),
 ( #12718, #7476 ),
 ( #11218, #2111 ) ),
 .UNSPECIFIED., .F., .F., .F.,
 ( 4, 4 ),
 ( 2, 2 ),
 ( 0.000000000000000000, 0.8452273900860258760 ),
 ( 0.000000000000000000, 1.000000000000000000 ),
 .UNSPECIFIED. ) ;
#11607 = ORIENTED_EDGE ( 'NONE', *, *, #10708, .F. ) ;
#11608 = ORIENTED_EDGE ( 'NONE', *, *, #13322, .T. ) ;
#11609 = ORIENTED_EDGE ( 'NONE', *, *, #9016, .T. ) ;
#11610 = PLANE ( 'NONE',  #6185 ) ;
#11611 = LINE ( 'NONE', #9466, #3176 ) ;
#11612 = CARTESIAN_POINT ( 'NONE',  ( 5.250000000000000000, 0.000000000000000000, -29.44078293894052933 ) ) ;
#11613 = DIRECTION ( 'NONE',  ( 0.000000000000000000, 1.000000000000000000, -0.000000000000000000 ) ) ;
#11614 = FACE_OUTER_BOUND ( 'NONE', #5396, .T. ) ;
#11615 = DIRECTION ( 'NONE',  ( 0.000000000000000000, 0.000000000000000000, 1.000000000000000000 ) ) ;
#11616 = VERTEX_POINT ( 'NONE', #7822 ) ;
#11617 = ADVANCED_FACE ( 'NONE', ( #2730 ), #5541, .F. ) ;
#11618 = PRODUCT_DEFINITION ( 'UNKNOWN', '', #1907, #3917 ) ;
#11619 = ORIENTED_EDGE ( 'NONE', *, *, #2207, .T. ) ;
#11620 = B_SPLINE_SURFACE_WITH_KNOTS ( 'NONE', 3, 1, ( 
 ( #5083, #2747 ),
 ( #2951, #11362 ),
 ( #1988, #823 ),
 ( #6121, #958 ) ),
 .UNSPECIFIED., .F., .F., .F.,
 ( 4, 4 ),
 ( 2, 2 ),
 ( 0.000000000000000000, 0.8452273900860258760 ),
 ( 0.000000000000000000, 1.000000000000000000 ),
 .UNSPECIFIED. ) ;
#11621 = DIRECTION ( 'NONE',  ( -0.000000000000000000, -1.000000000000000000, -0.000000000000000000 ) ) ;
#11622 = ORIENTED_EDGE ( 'NONE', *, *, #12061, .F. ) ;
#11623 = FACE_OUTER_BOUND ( 'NONE', #13074, .T. ) ;
#11624 = CARTESIAN_POINT ( 'NONE',  ( 0.000000000000000000, 3.000000000000000000, 0.000000000000000000 ) ) ;
#11625 = CARTESIAN_POINT ( 'NONE',  ( 30.66173999750687784, 3.000000000000000000, 0.01003121477750366919 ) ) ;
#11626 = FACE_OUTER_BOUND ( 'NONE', #6865, .T. ) ;
#11627 = CIRCLE ( 'NONE', #10750, 6.750000000000000888 ) ;
#11628 = CARTESIAN_POINT ( 'NONE',  ( -11.46847481510586775, 3.000000000000000000, -5.708888906988912382 ) ) ;
#11629 = ADVANCED_FACE ( 'NONE', ( #11139 ), #4674, .T. ) ;
#11630 = PLANE ( 'NONE',  #12463 ) ;
#11631 = EDGE_CURVE ( 'NONE', #3086, #12785, #1200, .T. ) ;
#11632 = CARTESIAN_POINT ( 'NONE',  ( 30.73000000000000043, 0.000000000000000000, -3.999999999999999112 ) ) ;
#11633 = ORIENTED_EDGE ( 'NONE', *, *, #5705, .F. ) ;
#11634 = ORIENTED_EDGE ( 'NONE', *, *, #2752, .F. ) ;
#11635 = EDGE_CURVE ( 'NONE', #12802, #7012, #3684, .T. ) ;
#11636 = ORIENTED_EDGE ( 'NONE', *, *, #4378, .T. ) ;
#11637 = CARTESIAN_POINT ( 'NONE',  ( -1.650143266773857142, 0.000000000000000000, -14.90895795148409952 ) ) ;
#11638 = ADVANCED_FACE ( 'NONE', ( #1433 ), #1370, .F. ) ;
#11639 = VERTEX_POINT ( 'NONE', #12997 ) ;
#11640 = CARTESIAN_POINT ( 'NONE',  ( 0.000000000000000000, 3.000000000000000000, 0.000000000000000000 ) ) ;
#11641 = CARTESIAN_POINT ( 'NONE',  ( 5.708888906988906164, 3.000000000000000000, -11.46847481510586775 ) ) ;
#11642 = CARTESIAN_POINT ( 'NONE',  ( 0.000000000000000000, 0.000000000000000000, 0.000000000000000000 ) ) ;
#11643 = CYLINDRICAL_SURFACE ( 'NONE', #6818, 14.25000000000000000 ) ;
#11644 = ADVANCED_FACE ( 'NONE', ( #10993 ), #6472, .T. ) ;
#11645 = CARTESIAN_POINT ( 'NONE',  ( 8.922136023539611216, 0.000000000000000000, -8.158651161643899030 ) ) ;
#11646 = FACE_OUTER_BOUND ( 'NONE', #10037, .T. ) ;
#11647 = ORIENTED_EDGE ( 'NONE', *, *, #5069, .F. ) ;
#11648 = VERTEX_POINT ( 'NONE', #4735 ) ;
#11649 = ORIENTED_EDGE ( 'NONE', *, *, #7355, .T. ) ;
#11650 = VECTOR ( 'NONE', #7699, 1000.000000000000000 ) ;
#11651 = ORIENTED_EDGE ( 'NONE', *, *, #1015, .T. ) ;
#11652 = CARTESIAN_POINT ( 'NONE',  ( 7.146769547044127258, 9.000000000000000000, -1.771712133291270863 ) ) ;
#11653 = ADVANCED_FACE ( 'NONE', ( #1641 ), #8415, .T. ) ;
#11654 = ORIENTED_EDGE ( 'NONE', *, *, #1102, .F. ) ;
#11655 = CARTESIAN_POINT ( 'NONE',  ( -12.55526518755974585, 0.000000000000000000, -2.546103534247746047 ) ) ;
#11656 = DIRECTION ( 'NONE',  ( 0.000000000000000000, 0.000000000000000000, 1.000000000000000000 ) ) ;
#11657 = CARTESIAN_POINT ( 'NONE',  ( 31.00000000000000000, 0.000000000000000000, -1.500000000759764029 ) ) ;
#11658 = VECTOR ( 'NONE', #12446, 1000.000000000000000 ) ;
#11659 = CARTESIAN_POINT ( 'NONE',  ( -12.76342233970728124, 0.000000000000000000, -4.564691384634500970 ) ) ;
#11660 = DIRECTION ( 'NONE',  ( 0.000000000000000000, 1.000000000000000000, -0.000000000000000000 ) ) ;
#11661 = EDGE_CURVE ( 'NONE', #1061, #3195, #8898, .T. ) ;
#11662 = CARTESIAN_POINT ( 'NONE',  ( 0.000000000000000000, 3.000000000000000000, 0.000000000000000000 ) ) ;
#11663 = EDGE_CURVE ( 'NONE', #8976, #11033, #3309, .T. ) ;
#11664 = CARTESIAN_POINT ( 'NONE',  ( 4.690415759823430619, 0.09999999999999982514, 1.500000000000000000 ) ) ;
#11665 = ORIENTED_EDGE ( 'NONE', *, *, #4725, .F. ) ;
#11666 = LINE ( 'NONE', #6499, #2690 ) ;
#11667 = ORIENTED_EDGE ( 'NONE', *, *, #2447, .F. ) ;
#11668 = ORIENTED_EDGE ( 'NONE', *, *, #125, .F. ) ;
#11669 = CIRCLE ( 'NONE', #7049, 3.000000000000000000 ) ;
#11670 = CIRCLE ( 'NONE', #5715, 1.500000000000003997 ) ;
#11671 = ORIENTED_EDGE ( 'NONE', *, *, #5862, .T. ) ;
#11672 = DIRECTION ( 'NONE',  ( 0.000000000000000000, 1.000000000000000000, 0.000000000000000000 ) ) ;
#11673 = DIRECTION ( 'NONE',  ( -0.000000000000000000, -1.000000000000000000, 0.000000000000000000 ) ) ;
#11674 = CARTESIAN_POINT ( 'NONE',  ( 26.30958424017656938, 3.000000000000000000, 4.500000000000000888 ) ) ;
#11675 = VECTOR ( 'NONE', #6122, 1000.000000000000000 ) ;
#11676 = CARTESIAN_POINT ( 'NONE',  ( 11.70905276178455878, 3.000000000000000000, -9.375397774054460953 ) ) ;
#11677 = FACE_OUTER_BOUND ( 'NONE', #42, .T. ) ;
#11678 = AXIS2_PLACEMENT_3D ( 'NONE', #6723, #4450, #6584 ) ;
#11679 = CARTESIAN_POINT ( 'NONE',  ( -12.08646469655240097, 0.000000000000000000, -8.883544964651921561 ) ) ;
#11680 = VERTEX_POINT ( 'NONE', #12640 ) ;
#11681 = VERTEX_POINT ( 'NONE', #9057 ) ;
#11682 = FACE_OUTER_BOUND ( 'NONE', #12725, .T. ) ;
#11683 = AXIS2_PLACEMENT_3D ( 'NONE', #9610, #186, #9810 ) ;
#11684 = AXIS2_PLACEMENT_3D ( 'NONE', #10978, #6712, #7614 ) ;
#11685 = VERTEX_POINT ( 'NONE', #11664 ) ;
#11686 = CARTESIAN_POINT ( 'NONE',  ( 47.14458624375820506, 0.000000000000000000, -3.829406728833672613 ) ) ;
#11687 = B_SPLINE_CURVE_WITH_KNOTS ( 'NONE', 2,
 ( #11087, #7839, #556 ),
 .UNSPECIFIED., .F., .F.,
 ( 3, 3 ),
 ( 0.000000000000000000, 1.000000000000000000 ),
 .UNSPECIFIED. ) ;
#11688 = EDGE_CURVE ( 'NONE', #1091, #5675, #12515, .T. ) ;
#11689 = CARTESIAN_POINT ( 'NONE',  ( 31.00000000000000000, 3.000000000000000000, -1.073670993220974656E-09 ) ) ;
#11690 = CARTESIAN_POINT ( 'NONE',  ( 0.000000000000000000, 0.000000000000000000, 1.399999999999999911 ) ) ;
#11691 = CARTESIAN_POINT ( 'NONE',  ( 2.604531154829233586, 3.000000000000000000, 11.80612203322752585 ) ) ;
#11692 = CARTESIAN_POINT ( 'NONE',  ( 49.72134184781355515, 0.000000000000000000, -3.261665100124877981 ) ) ;
#11693 = CARTESIAN_POINT ( 'NONE',  ( 8.208497377870823897, 0.000000000000000000, -5.549999999999999822 ) ) ;
#11694 = CARTESIAN_POINT ( 'NONE',  ( 3.647599401157691101, 3.000000000000000000, 11.52662650599084238 ) ) ;
#11695 = ORIENTED_EDGE ( 'NONE', *, *, #9606, .F. ) ;
#11696 = B_SPLINE_CURVE_WITH_KNOTS ( 'NONE', 3,
 ( #2765, #13030, #1529, #3790 ),
 .UNSPECIFIED., .F., .F.,
 ( 4, 4 ),
 ( 0.9090903094065657664, 0.9385083864668765097 ),
 .UNSPECIFIED. ) ;
#11697 = ORIENTED_EDGE ( 'NONE', *, *, #11346, .T. ) ;
#11698 = ORIENTED_EDGE ( 'NONE', *, *, #4536, .F. ) ;
#11699 = CARTESIAN_POINT ( 'NONE',  ( -2.161962830978783057, 3.000000000000000000, -14.08504230442586369 ) ) ;
#11700 = ORIENTED_EDGE ( 'NONE', *, *, #3801, .T. ) ;
#11701 = AXIS2_PLACEMENT_3D ( 'NONE', #11011, #9977, #9903 ) ;
#11702 = EDGE_CURVE ( 'NONE', #4625, #3023, #2529, .T. ) ;
#11703 = ADVANCED_FACE ( 'NONE', ( #8034, #37 ), #12706, .T. ) ;
#11704 = DIRECTION ( 'NONE',  ( 0.000000000000000000, 0.000000000000000000, 1.000000000000000000 ) ) ;
#11705 = B_SPLINE_SURFACE_WITH_KNOTS ( 'NONE', 3, 1, ( 
 ( #10167, #13552 ),
 ( #4107, #744 ),
 ( #1846, #5006 ),
 ( #9139, #11277 ) ),
 .UNSPECIFIED., .F., .F., .F.,
 ( 4, 4 ),
 ( 2, 2 ),
 ( 0.000000000000000000, 0.8452273900860258760 ),
 ( 0.000000000000000000, 1.000000000000000000 ),
 .UNSPECIFIED. ) ;
#11706 = CARTESIAN_POINT ( 'NONE',  ( 5.452638258930520010, 0.000000000000000000, -13.97385902380752754 ) ) ;
#11707 = CARTESIAN_POINT ( 'NONE',  ( 0.000000000000000000, 3.000000000000000000, 0.000000000000000000 ) ) ;
#11708 = CARTESIAN_POINT ( 'NONE',  ( -8.222660081691577361, 3.000000000000000000, -5.549999999999999822 ) ) ;
#11709 = EDGE_CURVE ( 'NONE', #672, #4801, #12571, .T. ) ;
#11710 = CARTESIAN_POINT ( 'NONE',  ( -6.017756925049793537, 0.000000000000000000, -11.52330688609026232 ) ) ;
#11711 = CARTESIAN_POINT ( 'NONE',  ( -11.70905276178464050, 0.000000000000000000, -9.375397774054366806 ) ) ;
#11712 = ORIENTED_EDGE ( 'NONE', *, *, #2446, .F. ) ;
#11713 = CIRCLE ( 'NONE', #6870, 8.500000000000000000 ) ;
#11714 = CARTESIAN_POINT ( 'NONE',  ( -11.11702303352197063, 3.000000000000000000, -8.914835885878215294 ) ) ;
#11715 = ORIENTED_EDGE ( 'NONE', *, *, #8172, .F. ) ;
#11716 = VECTOR ( 'NONE', #9178, 1000.000000000000000 ) ;
#11717 = AXIS2_PLACEMENT_3D ( 'NONE', #9724, #6629, #10832 ) ;
#11718 = VERTEX_POINT ( 'NONE', #7262 ) ;
#11719 = ORIENTED_EDGE ( 'NONE', *, *, #5835, .T. ) ;
#11720 = CARTESIAN_POINT ( 'NONE',  ( 5.571313494980132397, 0.000000000000000000, -10.72979803820131472 ) ) ;
#11721 = EDGE_LOOP ( 'NONE', ( #10620, #3442, #1661, #1197 ) ) ;
#11722 = EDGE_CURVE ( 'NONE', #2097, #1662, #2094, .T. ) ;
#11723 = B_SPLINE_CURVE_WITH_KNOTS ( 'NONE', 3,
 ( #8305, #1851, #10252, #11559 ),
 .UNSPECIFIED., .F., .F.,
 ( 4, 4 ),
 ( 0.000000000000000000, 0.8724294488011777871 ),
 .UNSPECIFIED. ) ;
#11724 = DIRECTION ( 'NONE',  ( 0.000000000000000000, 0.000000000000000000, -1.000000000000000000 ) ) ;
#11725 = CIRCLE ( 'NONE', #3353, 12.08999999999737440 ) ;
#11726 = CARTESIAN_POINT ( 'NONE',  ( 9.325031192972383920, 0.000000000000000000, -9.065266643391169055 ) ) ;
#11727 = AXIS2_PLACEMENT_3D ( 'NONE', #12318, #10243, #13349 ) ;
#11728 = AXIS2_PLACEMENT_3D ( 'NONE', #2478, #3371, #3499 ) ;
#11729 = CARTESIAN_POINT ( 'NONE',  ( -12.51336114795298471, 3.000000000000000000, -3.542894103880322998 ) ) ;
#11730 = CARTESIAN_POINT ( 'NONE',  ( 7.771282357155271825, 0.000000000000000000, -3.443424244174282389 ) ) ;
#11731 = FACE_BOUND ( 'NONE', #4079, .T. ) ;
#11732 = EDGE_CURVE ( 'NONE', #899, #2380, #11399, .T. ) ;
#11733 = DIRECTION ( 'NONE',  ( 0.000000000000000000, 0.000000000000000000, 1.000000000000000000 ) ) ;
#11734 = EDGE_CURVE ( 'NONE', #8800, #8278, #2746, .T. ) ;
#11735 = CARTESIAN_POINT ( 'NONE',  ( 26.30958424017656938, 3.000000000000000000, 1.500000000000000000 ) ) ;
#11736 = DIRECTION ( 'NONE',  ( 0.000000000000000000, 0.000000000000000000, -1.000000000000000000 ) ) ;
#11737 = VERTEX_POINT ( 'NONE', #6425 ) ;
#11738 = CARTESIAN_POINT ( 'NONE',  ( -13.27898586450066709, 0.000000000000000000, 5.170206418547661720 ) ) ;
#11739 = ORIENTED_EDGE ( 'NONE', *, *, #3867, .T. ) ;
#11740 = VECTOR ( 'NONE', #1913, 1000.000000000000000 ) ;
#11741 = ORIENTED_EDGE ( 'NONE', *, *, #11927, .F. ) ;
#11742 = AXIS2_PLACEMENT_3D ( 'NONE', #7200, #2156, #9395 ) ;
#11743 =( GEOMETRIC_REPRESENTATION_CONTEXT ( 3 ) GLOBAL_UNCERTAINTY_ASSIGNED_CONTEXT ( ( #13433 ) ) GLOBAL_UNIT_ASSIGNED_CONTEXT ( ( #5357, #10930, #11142 ) ) REPRESENTATION_CONTEXT ( 'NONE', 'WORKASPACE' ) );
#11744 = ORIENTED_EDGE ( 'NONE', *, *, #2516, .F. ) ;
#11745 = FACE_OUTER_BOUND ( 'NONE', #8157, .T. ) ;
#11746 = CARTESIAN_POINT ( 'NONE',  ( 2.601737331980797041, -1.694065894508600678E-18, -6.888123234756056590 ) ) ;
#11747 = AXIS2_PLACEMENT_3D ( 'NONE', #5400, #241, #12914 ) ;
#11748 = CARTESIAN_POINT ( 'NONE',  ( -6.749999880766614169, 0.000000000000000000, -0.001268720102703522860 ) ) ;
#11749 = CIRCLE ( 'NONE', #9105, 0.1000000000000000472 ) ;
#11750 = CARTESIAN_POINT ( 'NONE',  ( 5.452638258930520010, 0.000000000000000000, -13.97385902380752754 ) ) ;
#11751 = CARTESIAN_POINT ( 'NONE',  ( -12.08646469655240097, 3.000000000000000000, -8.883544964651921561 ) ) ;
#11752 = DIRECTION ( 'NONE',  ( -1.000000000000000000, 0.000000000000000000, 0.000000000000000000 ) ) ;
#11753 = ORIENTED_EDGE ( 'NONE', *, *, #531, .T. ) ;
#11754 = ORIENTED_EDGE ( 'NONE', *, *, #8881, .F. ) ;
#11755 = DIRECTION ( 'NONE',  ( -0.000000000000000000, -1.000000000000000000, -0.000000000000000000 ) ) ;
#11756 = VECTOR ( 'NONE', #875, 1000.000000000000000 ) ;
#11757 = AXIS2_PLACEMENT_3D ( 'NONE', #4810, #10107, #7899 ) ;
#11758 = CIRCLE ( 'NONE', #9556, 2.999999999999999112 ) ;
#11759 = ORIENTED_EDGE ( 'NONE', *, *, #2554, .F. ) ;
#11760 = DIRECTION ( 'NONE',  ( 0.000000000000000000, 0.000000000000000000, 1.000000000000000000 ) ) ;
#11761 = CARTESIAN_POINT ( 'NONE',  ( 6.509732753943064054, 9.000000000000000000, -3.441899519755141412 ) ) ;
#11762 = DIRECTION ( 'NONE',  ( -0.7772490812545725936, 0.000000000000000000, -0.6291930273683289387 ) ) ;
#11763 = CARTESIAN_POINT ( 'NONE',  ( -6.017756925049793537, 3.000000000000000000, -11.52330688609026232 ) ) ;
#11764=STYLED_ITEM('',(#13628),#13416);
#11765 = CARTESIAN_POINT ( 'NONE',  ( 0.7944557581062196006, 9.000000000000000000, -6.703084368289862205 ) ) ;
#11766 = CIRCLE ( 'NONE', #4066, 3.499999999999999556 ) ;
#11767 = CARTESIAN_POINT ( 'NONE',  ( 51.38094353598858532, 3.000000000000000000, -3.436371243710653722 ) ) ;
#11768 = VECTOR ( 'NONE', #2284, 1000.000000000000114 ) ;
#11769 = CARTESIAN_POINT ( 'NONE',  ( 0.7702044561450380744, 0.000000000000000000, -12.79759916868914615 ) ) ;
#11770 = EDGE_LOOP ( 'NONE', ( #8941, #3373, #5600, #947, #5025, #806, #8371, #4764, #12736, #9310, #3949, #10533, #7535, #11997, #8533, #3858, #4518, #12898, #13090, #4563, #10933, #8118, #7827, #6692, #3661, #3177, #8583, #4960, #7041, #4123, #10723, #9859, #2788, #10173, #1931, #6869, #6503, #6155, #1572, #3434, #10234, #6995, #8200, #6945, #10657, #1717, #12641, #8203, #401, #11533, #10054, #7387, #2856, #7678, #12713, #8042, #9800, #12678, #149, #12970, #12382, #4414, #7908, #410, #7283, #5563, #11018, #10692, #3616, #11609, #7565, #8989, #4008, #5574, #7313, #13055, #9411, #11671, #163, #8977, #399, #1487, #5410, #8620, #340, #11849, #2719, #11058, #11387, #3452, #9455 ) ) ;
#11771 = ORIENTED_EDGE ( 'NONE', *, *, #8334, .T. ) ;
#11772 = ORIENTED_EDGE ( 'NONE', *, *, #6943, .F. ) ;
#11773 = DIRECTION ( 'NONE',  ( 0.000000000000000000, 1.000000000000000000, 0.000000000000000000 ) ) ;
#11774 = ORIENTED_EDGE ( 'NONE', *, *, #11273, .F. ) ;
#11775 = VECTOR ( 'NONE', #2458, 1000.000000000000227 ) ;
#11776 = CARTESIAN_POINT ( 'NONE',  ( 9.325031192972383920, 3.000000000000000000, -9.065266643391169055 ) ) ;
#11777 = CARTESIAN_POINT ( 'NONE',  ( 45.60964950616533287, 3.000000000000000000, -14.50984893380129392 ) ) ;
#11778 = DIRECTION ( 'NONE',  ( 0.000000000000000000, 0.000000000000000000, 1.000000000000000000 ) ) ;
#11779 = DIRECTION ( 'NONE',  ( 0.000000000000000000, 0.000000000000000000, -1.000000000000000000 ) ) ;
#11780 = CYLINDRICAL_SURFACE ( 'NONE', #10595, 3.499999999999999556 ) ;
#11781 = CARTESIAN_POINT ( 'NONE',  ( 0.000000000000000000, 3.000000000000000000, 0.000000000000000000 ) ) ;
#11782 = B_SPLINE_CURVE_WITH_KNOTS ( 'NONE', 3,
 ( #6976, #7857, #7042, #13241 ),
 .UNSPECIFIED., .F., .F.,
 ( 4, 4 ),
 ( 0.000000000000000000, 0.5855695330273008592 ),
 .UNSPECIFIED. ) ;
#11783 = ORIENTED_EDGE ( 'NONE', *, *, #11960, .F. ) ;
#11784 =( GEOMETRIC_REPRESENTATION_CONTEXT ( 3 ) GLOBAL_UNCERTAINTY_ASSIGNED_CONTEXT ( ( #13157 ) ) GLOBAL_UNIT_ASSIGNED_CONTEXT ( ( #835, #3712, #13440 ) ) REPRESENTATION_CONTEXT ( 'NONE', 'WORKASPACE' ) );
#11785 = CARTESIAN_POINT ( 'NONE',  ( -14.16466328168010769, 3.000000000000000000, -1.557181465540673271 ) ) ;
#11786 = EDGE_LOOP ( 'NONE', ( #7931, #4137, #12578, #2595 ) ) ;
#11787 = ORIENTED_EDGE ( 'NONE', *, *, #24, .T. ) ;
#11788 = EDGE_CURVE ( 'NONE', #1501, #6519, #3288, .T. ) ;
#11789 = PRODUCT_RELATED_PRODUCT_CATEGORY ( 'part', '', ( #5568 ) ) ;
#11790 = ORIENTED_EDGE ( 'NONE', *, *, #935, .T. ) ;
#11791 = DIRECTION ( 'NONE',  ( -0.000000000000000000, -1.000000000000000000, -0.000000000000000000 ) ) ;
#11792 = VERTEX_POINT ( 'NONE', #4153 ) ;
#11793 = ORIENTED_EDGE ( 'NONE', *, *, #12636, .T. ) ;
#11794 = CARTESIAN_POINT ( 'NONE',  ( 13.27898586450067242, 3.000000000000000000, -5.170206418547655502 ) ) ;
#11795 = ORIENTED_EDGE ( 'NONE', *, *, #7, .T. ) ;
#11796 = PRESENTATION_STYLE_ASSIGNMENT (( #9848 ) ) ;
#11797 = DIRECTION ( 'NONE',  ( -0.000000000000000000, -1.000000000000000000, 0.000000000000000000 ) ) ;
#11798 = FACE_OUTER_BOUND ( 'NONE', #9170, .T. ) ;
#11799 = CARTESIAN_POINT ( 'NONE',  ( 2.161962830978694683, 3.000000000000000000, -14.08504230442587790 ) ) ;
#11800 = CYLINDRICAL_SURFACE ( 'NONE', #4435, 2.500000000000000444 ) ;
#11801 = CARTESIAN_POINT ( 'NONE',  ( 31.00000000000000000, 3.000000000000000000, 0.000000000000000000 ) ) ;
#11802 = ORIENTED_EDGE ( 'NONE', *, *, #4817, .T. ) ;
#11803 = CARTESIAN_POINT ( 'NONE',  ( 6.343080161942737938, 3.000000000000000000, -11.35348358516942469 ) ) ;
#11804 = EDGE_CURVE ( 'NONE', #4379, #2013, #10637, .T. ) ;
#11805 = ORIENTED_EDGE ( 'NONE', *, *, #5806, .F. ) ;
#11806 = EDGE_CURVE ( 'NONE', #10001, #7949, #7594, .T. ) ;
#11807 = VERTEX_POINT ( 'NONE', #1126 ) ;
#11808 = EDGE_CURVE ( 'NONE', #10780, #2104, #8245, .T. ) ;
#11809 = ORIENTED_EDGE ( 'NONE', *, *, #11663, .F. ) ;
#11810 = EDGE_CURVE ( 'NONE', #10891, #4765, #5198, .T. ) ;
#11811 = ADVANCED_FACE ( 'NONE', ( #8346 ), #3115, .F. ) ;
#11812 = B_SPLINE_CURVE_WITH_KNOTS ( 'NONE', 3,
 ( #1177, #12888, #12621, #10544 ),
 .UNSPECIFIED., .F., .F.,
 ( 4, 4 ),
 ( 0.000000000000000000, 0.8724294488011768989 ),
 .UNSPECIFIED. ) ;
#11813 = FACE_BOUND ( 'NONE', #5870, .T. ) ;
#11814 = CARTESIAN_POINT ( 'NONE',  ( 6.217402469309262436, 0.000000000000000000, -13.03533457366732939 ) ) ;
#11815 = CARTESIAN_POINT ( 'NONE',  ( 53.78299299645824050, 3.000000000000000000, -4.528231303176834643 ) ) ;
#11816 = CARTESIAN_POINT ( 'NONE',  ( 8.795158114916441505, 0.000000000000000000, -9.573149624528689117 ) ) ;
#11817 = DIRECTION ( 'NONE',  ( 0.000000000000000000, 0.000000000000000000, 1.000000000000000000 ) ) ;
#11818 = DIRECTION ( 'NONE',  ( 0.000000000000000000, 0.000000000000000000, 1.000000000000000000 ) ) ;
#11819 = EDGE_CURVE ( 'NONE', #375, #3649, #1398, .T. ) ;
#11820 = ORIENTED_EDGE ( 'NONE', *, *, #13209, .T. ) ;
#11821 = ORIENTED_EDGE ( 'NONE', *, *, #3460, .T. ) ;
#11822 = CARTESIAN_POINT ( 'NONE',  ( 8.922226997226887946, 0.000000000000000000, 8.158551673544288008 ) ) ;
#11823 = B_SPLINE_SURFACE_WITH_KNOTS ( 'NONE', 3, 1, ( 
 ( #9608, #12779 ),
 ( #184, #380 ),
 ( #6571, #5670 ),
 ( #4436, #10712 ) ),
 .UNSPECIFIED., .F., .F., .F.,
 ( 4, 4 ),
 ( 2, 2 ),
 ( 0.000000000000000000, 0.8724294488011786752 ),
 ( 0.000000000000000000, 1.000000000000000000 ),
 .UNSPECIFIED. ) ;
#11824 = EDGE_CURVE ( 'NONE', #4803, #2397, #12000, .T. ) ;
#11825 = ORIENTED_EDGE ( 'NONE', *, *, #13564, .T. ) ;
#11826 = CARTESIAN_POINT ( 'NONE',  ( -8.914835885878215294, 3.000000000000000000, 11.11702303352197063 ) ) ;
#11827 = CYLINDRICAL_SURFACE ( 'NONE', #11225, 8.499999999999996447 ) ;
#11828 = DIRECTION ( 'NONE',  ( -0.000000000000000000, -1.000000000000000000, -0.000000000000000000 ) ) ;
#11829 = DIRECTION ( 'NONE',  ( -0.000000000000000000, -1.000000000000000000, -0.000000000000000000 ) ) ;
#11830 = CARTESIAN_POINT ( 'NONE',  ( 9.250000000000001776, 2.000000000000000000, 10.00000000000000000 ) ) ;
#11831 = CARTESIAN_POINT ( 'NONE',  ( 13.27898586450067420, 0.000000000000000000, 5.170206418547648397 ) ) ;
#11832 = EDGE_CURVE ( 'NONE', #3124, #11905, #11357, .T. ) ;
#11833 = CARTESIAN_POINT ( 'NONE',  ( -13.73660796332618261, 0.000000000000000000, -6.025412986832017204 ) ) ;
#11834 = ADVANCED_FACE ( 'NONE', ( #3451 ), #174, .T. ) ;
#11835 = CARTESIAN_POINT ( 'NONE',  ( 8.158651161643900807, 3.000000000000000000, 8.922136023539609440 ) ) ;
#11836 = ORIENTED_EDGE ( 'NONE', *, *, #12219, .T. ) ;
#11837 = ORIENTED_EDGE ( 'NONE', *, *, #11123, .T. ) ;
#11838 = VERTEX_POINT ( 'NONE', #8748 ) ;
#11839 = VERTEX_POINT ( 'NONE', #10964 ) ;
#11840 = DIRECTION ( 'NONE',  ( 0.000000000000000000, 0.000000000000000000, 1.000000000000000000 ) ) ;
#11841 = EDGE_CURVE ( 'NONE', #9010, #5996, #5380, .T. ) ;
#11842 = ORIENTED_EDGE ( 'NONE', *, *, #4467, .T. ) ;
#11843 = CARTESIAN_POINT ( 'NONE',  ( -6.025412986832177076, 0.000000000000000000, -13.73660796332610268 ) ) ;
#11844 = CARTESIAN_POINT ( 'NONE',  ( 7.659717769608228366, 9.000000000000000000, -2.099897208369672530 ) ) ;
#11845 = FACE_OUTER_BOUND ( 'NONE', #7849, .T. ) ;
#11846 = PRODUCT_DEFINITION_SHAPE ( 'NONE', 'NONE',  #13609 ) ;
#11847 = CARTESIAN_POINT ( 'NONE',  ( -6.721397655168932062, 9.000000000000000000, 5.203154193476253297 ) ) ;
#11848 = CARTESIAN_POINT ( 'NONE',  ( 0.000000000000000000, 3.000000000000000000, 0.000000000000000000 ) ) ;
#11849 = ORIENTED_EDGE ( 'NONE', *, *, #5007, .T. ) ;
#11850 = CARTESIAN_POINT ( 'NONE',  ( -13.28140389626389783, 3.000000000000000000, 0.000000000000000000 ) ) ;
#11851 = VERTEX_POINT ( 'NONE', #8614 ) ;
#11852 = ORIENTED_EDGE ( 'NONE', *, *, #1952, .T. ) ;
#11853 = ORIENTED_EDGE ( 'NONE', *, *, #11291, .F. ) ;
#11854 = CARTESIAN_POINT ( 'NONE',  ( 10.00000000000001599, 6.750000000000007105, -2.770445225425678767E-15 ) ) ;
#11855 = ORIENTED_EDGE ( 'NONE', *, *, #9212, .F. ) ;
#11856 = ORIENTED_EDGE ( 'NONE', *, *, #5677, .T. ) ;
#11857 = CARTESIAN_POINT ( 'NONE',  ( -13.73660796332618261, 3.000000000000000000, -6.025412986832017204 ) ) ;
#11858 =( LENGTH_UNIT ( ) NAMED_UNIT ( * ) SI_UNIT ( .MILLI., .METRE. ) );
#11859 = CARTESIAN_POINT ( 'NONE',  ( 6.000000000000008882, 3.000000000000000000, 27.00000000000000000 ) ) ;
#11860 = LINE ( 'NONE', #8543, #1770 ) ;
#11861 = EDGE_CURVE ( 'NONE', #1662, #2097, #5170, .T. ) ;
#11862 = DIRECTION ( 'NONE',  ( -0.000000000000000000, -1.000000000000000000, 0.000000000000000000 ) ) ;
#11863 = CARTESIAN_POINT ( 'NONE',  ( -0.8776997859584816375, 9.000000000000000000, 7.310603390113379341 ) ) ;
#11864 = CARTESIAN_POINT ( 'NONE',  ( -2.264806262022998062, 0.000000000000000000, -14.82803603298499340 ) ) ;
#11865 = ORIENTED_EDGE ( 'NONE', *, *, #13578, .T. ) ;
#11866 = CARTESIAN_POINT ( 'NONE',  ( 5.806472362263156661, 0.000000000000000000, -5.419014975255640465 ) ) ;
#11867 = ORIENTED_EDGE ( 'NONE', *, *, #8509, .T. ) ;
#11868 = ORIENTED_EDGE ( 'NONE', *, *, #11404, .F. ) ;
#11869 = ORIENTED_EDGE ( 'NONE', *, *, #10044, .T. ) ;
#11870 = AXIS2_PLACEMENT_3D ( 'NONE', #13359, #8046, #4871 ) ;
#11871 = DIRECTION ( 'NONE',  ( -0.000000000000000000, -1.000000000000000000, -0.000000000000000000 ) ) ;
#11872 = CARTESIAN_POINT ( 'NONE',  ( -14.82803603298498629, 3.000000000000000000, 2.264806262023049577 ) ) ;
#11873 = EDGE_CURVE ( 'NONE', #937, #12613, #6927, .T. ) ;
#11874 = EDGE_CURVE ( 'NONE', #4083, #10517, #550, .T. ) ;
#11875 = CARTESIAN_POINT ( 'NONE',  ( 13.50000000000000355, 0.000000000000000000, -7.050000000000000711 ) ) ;
#11876 = DIRECTION ( 'NONE',  ( 0.000000000000000000, 0.000000000000000000, -1.000000000000000000 ) ) ;
#11877 = CARTESIAN_POINT ( 'NONE',  ( 2.392396671352952087, 9.000000000000000000, 6.311809420990097230 ) ) ;
#11878 = CARTESIAN_POINT ( 'NONE',  ( -12.07794044664754018, 0.000000000000000000, -0.5398653231797256868 ) ) ;
#11879 = EDGE_CURVE ( 'NONE', #144, #2380, #1176, .T. ) ;
#11880 = CIRCLE ( 'NONE', #5065, 14.24999999999999822 ) ;
#11881 = AXIS2_PLACEMENT_3D ( 'NONE', #8409, #229, #3186 ) ;
#11882 = ORIENTED_EDGE ( 'NONE', *, *, #7094, .F. ) ;
#11883 = ORIENTED_EDGE ( 'NONE', *, *, #9788, .F. ) ;
#11884 = CARTESIAN_POINT ( 'NONE',  ( 8.208497377870823897, 3.000000000000000000, -5.549999999999999822 ) ) ;
#11885 = ORIENTED_EDGE ( 'NONE', *, *, #6175, .F. ) ;
#11886 = CARTESIAN_POINT ( 'NONE',  ( -14.87484884897978077, 3.000000000000000000, -1.958311002203079187 ) ) ;
#11887 = CARTESIAN_POINT ( 'NONE',  ( -20.56403552112892896, 3.000000000000000000, -16.70078978407140013 ) ) ;
#11888 = AXIS2_PLACEMENT_3D ( 'NONE', #2635, #8823, #2781 ) ;
#11889 = EDGE_CURVE ( 'NONE', #10564, #5245, #6561, .T. ) ;
#11890 = B_SPLINE_SURFACE_WITH_KNOTS ( 'NONE', 3, 1, ( 
 ( #5527, #9604 ),
 ( #2372, #6567 ),
 ( #182, #7667 ),
 ( #10768, #2432 ) ),
 .UNSPECIFIED., .F., .F., .F.,
 ( 4, 4 ),
 ( 2, 2 ),
 ( 0.1276832474596280298, 1.000000000000000000 ),
 ( 0.000000000000000000, 1.000000000000000000 ),
 .UNSPECIFIED. ) ;
#11891 = AXIS2_PLACEMENT_3D ( 'NONE', #3362, #12744, #11507 ) ;
#11892 = DIRECTION ( 'NONE',  ( 0.000000000000000000, 1.000000000000000000, -0.000000000000000000 ) ) ;
#11893 = LINE ( 'NONE', #1563, #5510 ) ;
#11894 = DIRECTION ( 'NONE',  ( 0.000000000000000000, 1.000000000000000000, 0.000000000000000000 ) ) ;
#11895 = DIRECTION ( 'NONE',  ( 1.000000000000000000, 0.000000000000000000, 0.000000000000000000 ) ) ;
#11896 = ADVANCED_FACE ( 'NONE', ( #8689 ), #7724, .F. ) ;
#11897 = DIRECTION ( 'NONE',  ( 0.000000000000000000, 0.000000000000000000, -1.000000000000000000 ) ) ;
#11898 = B_SPLINE_CURVE_WITH_KNOTS ( 'NONE', 3,
 ( #9300, #7179, #9226, #6267 ),
 .UNSPECIFIED., .F., .F.,
 ( 4, 4 ),
 ( 0.1276832474596280298, 1.000000000000000000 ),
 .UNSPECIFIED. ) ;
#11899 = CARTESIAN_POINT ( 'NONE',  ( -5.039625798601655937, 0.000000000000000000, 4.490509081392509927 ) ) ;
#11900 = ORIENTED_EDGE ( 'NONE', *, *, #7541, .F. ) ;
#11901 = VECTOR ( 'NONE', #12336, 1000.000000000000000 ) ;
#11902 = ORIENTED_EDGE ( 'NONE', *, *, #5070, .T. ) ;
#11903 = CIRCLE ( 'NONE', #11463, 1.500000000000000222 ) ;
#11904 = ORIENTED_EDGE ( 'NONE', *, *, #2231, .T. ) ;
#11905 = VERTEX_POINT ( 'NONE', #4360 ) ;
#11906 = CARTESIAN_POINT ( 'NONE',  ( -2.428572470324203980, 3.000000000000000000, -13.33579367773357482 ) ) ;
#11907 = VERTEX_POINT ( 'NONE', #12767 ) ;
#11908 = EDGE_CURVE ( 'NONE', #13228, #10765, #11766, .T. ) ;
#11909 = EDGE_CURVE ( 'NONE', #116, #6616, #7528, .T. ) ;
#11910 = DIRECTION ( 'NONE',  ( 0.000000000000000000, 0.000000000000000000, -1.000000000000000000 ) ) ;
#11911 = VECTOR ( 'NONE', #1686, 1000.000000000000000 ) ;
#11912 = DIRECTION ( 'NONE',  ( 0.000000000000000000, 0.000000000000000000, 1.000000000000000000 ) ) ;
#11913 = DIRECTION ( 'NONE',  ( 0.000000000000000000, 1.000000000000000000, 0.000000000000000000 ) ) ;
#11914 = DIRECTION ( 'NONE',  ( -0.000000000000000000, -1.000000000000000000, -0.000000000000000000 ) ) ;
#11915 = FACE_OUTER_BOUND ( 'NONE', #4364, .T. ) ;
#11916 = CARTESIAN_POINT ( 'NONE',  ( 51.41686768994642165, 3.000000000000000000, -11.86457109001525545 ) ) ;
#11917 = VERTEX_POINT ( 'NONE', #11864 ) ;
#11918 = CARTESIAN_POINT ( 'NONE',  ( 0.000000000000000000, 13.00000000000000178, 0.000000000000000000 ) ) ;
#11919 = VERTEX_POINT ( 'NONE', #12964 ) ;
#11920 = PRODUCT_DEFINITION_CONTEXT ( 'detailed design', #2041, 'design' ) ;
#11921 = ORIENTED_EDGE ( 'NONE', *, *, #4128, .T. ) ;
#11922 = CARTESIAN_POINT ( 'NONE',  ( 5.733772933379474246, 0.000000000000000000, -13.04554897075799502 ) ) ;
#11923 = AXIS2_PLACEMENT_3D ( 'NONE', #3927, #4972, #4197 ) ;
#11924 = VERTEX_POINT ( 'NONE', #9722 ) ;
#11925 = ADVANCED_FACE ( 'NONE', ( #3516 ), #4623, .F. ) ;
#11926 = VERTEX_POINT ( 'NONE', #13033 ) ;
#11927 = EDGE_CURVE ( 'NONE', #1592, #12572, #12012, .T. ) ;
#11928 = FACE_OUTER_BOUND ( 'NONE', #4046, .T. ) ;
#11929 =( LENGTH_UNIT ( ) NAMED_UNIT ( * ) SI_UNIT ( .MILLI., .METRE. ) );
#11930 = CARTESIAN_POINT ( 'NONE',  ( 2.414978278956333213, 3.000000000000000000, -13.33788847341978645 ) ) ;
#11931 = FACE_OUTER_BOUND ( 'NONE', #2888, .T. ) ;
#11932 = CARTESIAN_POINT ( 'NONE',  ( -14.82803603298498629, 0.000000000000000000, 2.264806262023049577 ) ) ;
#11933 = AXIS2_PLACEMENT_3D ( 'NONE', #12006, #5927, #6694 ) ;
#11934 = AXIS2_PLACEMENT_3D ( 'NONE', #4514, #3332, #11818 ) ;
#11935 = ADVANCED_FACE ( 'NONE', ( #8133 ), #12360, .F. ) ;
#11936 = DIRECTION ( 'NONE',  ( -0.000000000000000000, -1.000000000000000000, -0.000000000000000000 ) ) ;
#11937 = DIRECTION ( 'NONE',  ( 0.000000000000000000, 0.000000000000000000, 1.000000000000000000 ) ) ;
#11938 = ORIENTED_EDGE ( 'NONE', *, *, #9649, .T. ) ;
#11939 = CARTESIAN_POINT ( 'NONE',  ( -6.017756925049793537, 3.000000000000000000, -11.52330688609026232 ) ) ;
#11940 = B_SPLINE_SURFACE_WITH_KNOTS ( 'NONE', 3, 1, ( 
 ( #5372, #157 ),
 ( #8794, #9837 ),
 ( #13015, #7444 ),
 ( #4345, #11711 ) ),
 .UNSPECIFIED., .F., .F., .F.,
 ( 4, 4 ),
 ( 2, 2 ),
 ( 0.000000000000000000, 0.5855695330273008592 ),
 ( 0.000000000000000000, 1.000000000000000000 ),
 .UNSPECIFIED. ) ;
#11941 = VERTEX_POINT ( 'NONE', #496 ) ;
#11942 = ORIENTED_EDGE ( 'NONE', *, *, #3629, .T. ) ;
#11943 = VERTEX_POINT ( 'NONE', #13381 ) ;
#11944 = VECTOR ( 'NONE', #8401, 1000.000000000000000 ) ;
#11945 = VECTOR ( 'NONE', #12037, 1000.000000000000000 ) ;
#11946 = AXIS2_PLACEMENT_3D ( 'NONE', #1963, #4096, #3054 ) ;
#11947 = CARTESIAN_POINT ( 'NONE',  ( -2.411622991978541464, 0.000000000000000000, -6.304488444319688689 ) ) ;
#11948 = CARTESIAN_POINT ( 'NONE',  ( 9.573149624528804580, 0.000000000000000000, -8.795158114916638681 ) ) ;
#11949 = CARTESIAN_POINT ( 'NONE',  ( 3.647470871583629926, 3.000000000000000000, -11.52666717836884125 ) ) ;
#11950 = CARTESIAN_POINT ( 'NONE',  ( 10.69794375946289655, 0.000000000000000000, 7.065816209474157006 ) ) ;
#11951 = DIRECTION ( 'NONE',  ( 0.000000000000000000, 0.000000000000000000, 1.000000000000000000 ) ) ;
#11952 = DIRECTION ( 'NONE',  ( 0.000000000000000000, 1.000000000000000000, 0.000000000000000000 ) ) ;
#11953 = VECTOR ( 'NONE', #4535, 1000.000000000000000 ) ;
#11954 = CARTESIAN_POINT ( 'NONE',  ( 13.11311062740304401, 0.000000000000000000, -1.563624455674628377 ) ) ;
#11955 = AXIS2_PLACEMENT_3D ( 'NONE', #6989, #2710, #6915 ) ;
#11956 = AXIS2_PLACEMENT_3D ( 'NONE', #7904, #9980, #13091 ) ;
#11957 = ORIENTED_EDGE ( 'NONE', *, *, #2538, .T. ) ;
#11958 = ORIENTED_EDGE ( 'NONE', *, *, #9726, .F. ) ;
#11959 = ADVANCED_FACE ( 'NONE', ( #8072, #3928, #7117 ), #2692, .T. ) ;
#11960 = EDGE_CURVE ( 'NONE', #6054, #1237, #9130, .T. ) ;
#11961 = ORIENTED_EDGE ( 'NONE', *, *, #4321, .T. ) ;
#11962 = CARTESIAN_POINT ( 'NONE',  ( -8.482622935103766082, 3.000000000000000000, 9.600126836553263487 ) ) ;
#11963 = AXIS2_PLACEMENT_3D ( 'NONE', #5995, #64, #10458 ) ;
#11964 = PRODUCT_DEFINITION_SHAPE ( 'NONE', 'NONE',  #13597 ) ;
#11965 = CIRCLE ( 'NONE', #6031, 1.499999999999998668 ) ;
#11966 = CARTESIAN_POINT ( 'NONE',  ( 8.430890348300625448, 3.000000000000000000, 11.48836750521723893 ) ) ;
#11967 = LINE ( 'NONE', #8389, #11945 ) ;
#11968 = DIRECTION ( 'NONE',  ( 0.000000000000000000, 1.000000000000000000, -0.000000000000000000 ) ) ;
#11969 = CARTESIAN_POINT ( 'NONE',  ( -11.90209577080766046, 3.000000000000000000, -8.180229652970757215 ) ) ;
#11970 = CARTESIAN_POINT ( 'NONE',  ( 13.27898586450067242, 0.000000000000000000, -5.170206418547655502 ) ) ;
#11971 = CARTESIAN_POINT ( 'NONE',  ( 0.000000000000000000, 3.000000000000000000, 0.000000000000000000 ) ) ;
#11972 = VECTOR ( 'NONE', #2531, 1000.000000000000000 ) ;
#11973 = CARTESIAN_POINT ( 'NONE',  ( 51.83140210808490167, 3.000000000000000000, -12.77460472465662988 ) ) ;
#11974 = AXIS2_PLACEMENT_3D ( 'NONE', #1228, #5354, #8574 ) ;
#11975 = ORIENTED_EDGE ( 'NONE', *, *, #13471, .F. ) ;
#11976 = ADVANCED_FACE ( 'NONE', ( #2901 ), #1532, .F. ) ;
#11977 = ORIENTED_EDGE ( 'NONE', *, *, #11547, .F. ) ;
#11978 = ADVANCED_FACE ( 'NONE', ( #5718 ), #1607, .F. ) ;
#11979 = ORIENTED_EDGE ( 'NONE', *, *, #10971, .T. ) ;
#11980 = ORIENTED_EDGE ( 'NONE', *, *, #5758, .T. ) ;
#11981 = DIRECTION ( 'NONE',  ( -0.000000000000000000, -1.000000000000000000, -0.000000000000000000 ) ) ;
#11982 =( REPRESENTATION_RELATIONSHIP ('NONE','NONE', #3798, #5135 ) REPRESENTATION_RELATIONSHIP_WITH_TRANSFORMATION ( #7868 )SHAPE_REPRESENTATION_RELATIONSHIP( ) );
#11983 = ORIENTED_EDGE ( 'NONE', *, *, #1701, .F. ) ;
#11984 = ADVANCED_FACE ( 'NONE', ( #1676 ), #336, .T. ) ;
#11985 = EDGE_CURVE ( 'NONE', #2448, #1536, #3794, .T. ) ;
#11986 = CARTESIAN_POINT ( 'NONE',  ( 3.061616997868383634E-16, 0.000000000000000000, 2.500000000000000444 ) ) ;
#11987 = COLOUR_RGB ( '',0.7803921568627451011, 0.7607843137254901578, 0.7411764705882353255 ) ;
#11988 = FILL_AREA_STYLE ('',( #1369 ) ) ;
#11989 = AXIS2_PLACEMENT_3D ( 'NONE', #7293, #12603, #7166 ) ;
#11990 = CARTESIAN_POINT ( 'NONE',  ( -9.573149624528719315, 3.000000000000000000, -8.795158114916407754 ) ) ;
#11991 = CARTESIAN_POINT ( 'NONE',  ( 0.000000000000000000, 0.000000000000000000, 0.000000000000000000 ) ) ;
#11992 = DIRECTION ( 'NONE',  ( -0.000000000000000000, -1.000000000000000000, -0.000000000000000000 ) ) ;
#11993 = DIRECTION ( 'NONE',  ( -0.000000000000000000, -1.000000000000000000, -0.000000000000000000 ) ) ;
#11994 = CARTESIAN_POINT ( 'NONE',  ( -13.00394572736061605, 3.000000000000000000, 0.1835083749157108701 ) ) ;
#11995 = EDGE_LOOP ( 'NONE', ( #1313, #1187, #2804, #13093 ) ) ;
#11996 = EDGE_CURVE ( 'NONE', #9336, #7044, #1809, .T. ) ;
#11997 = ORIENTED_EDGE ( 'NONE', *, *, #11459, .T. ) ;
#11998 = STYLED_ITEM ( 'NONE', ( #11796 ), #10000 ) ;
#11999 = ORIENTED_EDGE ( 'NONE', *, *, #792, .T. ) ;
#12000 = CIRCLE ( 'NONE', #5603, 1.500000000000001332 ) ;
#12001 = CYLINDRICAL_SURFACE ( 'NONE', #7536, 6.750000000000000888 ) ;
#12002 = EDGE_LOOP ( 'NONE', ( #3027, #3133 ) ) ;
#12003 = ORIENTED_EDGE ( 'NONE', *, *, #2980, .T. ) ;
#12004 = CYLINDRICAL_SURFACE ( 'NONE', #9318, 0.9999999999999997780 ) ;
#12005 = SURFACE_STYLE_USAGE ( .BOTH. , #10820 ) ;
#12006 = CARTESIAN_POINT ( 'NONE',  ( 31.00000000000000000, 2.900000000000000355, 1.600000000000004086 ) ) ;
#12007 = CARTESIAN_POINT ( 'NONE',  ( 31.00000000000000000, 3.000000000000000000, -1.073670993220974656E-09 ) ) ;
#12008 = MECHANICAL_DESIGN_GEOMETRIC_PRESENTATION_REPRESENTATION (  '', ( #7172 ), #2764 ) ;
#12009 = CARTESIAN_POINT ( 'NONE',  ( -5.975392301194336397, 0.000000000000000000, -6.045220165289885372 ) ) ;
#12010 = VECTOR ( 'NONE', #9075, 1000.000000000000000 ) ;
#12011 = CARTESIAN_POINT ( 'NONE',  ( -14.82803603298502360, 0.000000000000000000, -2.264806262022826644 ) ) ;
#12012 = LINE ( 'NONE', #2293, #10451 ) ;
#12013 = EDGE_LOOP ( 'NONE', ( #3724, #12971, #5920, #4966 ) ) ;
#12014 = CARTESIAN_POINT ( 'NONE',  ( 29.39270799701850123, 0.000000000000000000, -0.3930766723116408401 ) ) ;
#12015 = EDGE_CURVE ( 'NONE', #7310, #11432, #8026, .T. ) ;
#12016 = ORIENTED_EDGE ( 'NONE', *, *, #5793, .T. ) ;
#12017 = EDGE_CURVE ( 'NONE', #6431, #12350, #11028, .T. ) ;
#12018 = B_SPLINE_CURVE_WITH_KNOTS ( 'NONE', 3,
 ( #5830, #1707, #6858, #8982 ),
 .UNSPECIFIED., .F., .F.,
 ( 4, 4 ),
 ( 0.000000000000000000, 0.8452273900860258760 ),
 .UNSPECIFIED. ) ;
#12019 = ORIENTED_EDGE ( 'NONE', *, *, #3527, .T. ) ;
#12020 = B_SPLINE_CURVE_WITH_KNOTS ( 'NONE', 3,
 ( #6545, #12748, #3433, #7644 ),
 .UNSPECIFIED., .F., .F.,
 ( 4, 4 ),
 ( 0.000000000000000000, 0.5855695330273008592 ),
 .UNSPECIFIED. ) ;
#12021 = ORIENTED_EDGE ( 'NONE', *, *, #5398, .T. ) ;
#12022 = LINE ( 'NONE', #10502, #8834 ) ;
#12023 = CARTESIAN_POINT ( 'NONE',  ( 12.48034623170854474, 3.000000000000000000, 4.337627373772809491 ) ) ;
#12024 = CARTESIAN_POINT ( 'NONE',  ( 51.38094353598858532, 3.000000000000000000, -3.436371243710653722 ) ) ;
#12025 = CARTESIAN_POINT ( 'NONE',  ( -12.98835496148299207, 3.000000000000000000, 0.5501230721524459355 ) ) ;
#12026 = CARTESIAN_POINT ( 'NONE',  ( -0.5501230721523990841, 3.000000000000000000, -12.98835496148299384 ) ) ;
#12027 = ITEM_DEFINED_TRANSFORMATION ( 'NONE', 'NONE', #8045,  #10007 ) ;
#12028 = FACE_OUTER_BOUND ( 'NONE', #12148, .T. ) ;
#12029 = CARTESIAN_POINT ( 'NONE',  ( -9.324917476840782982, 3.000000000000000000, -9.065441278446241924 ) ) ;
#12030 = CARTESIAN_POINT ( 'NONE',  ( 5.571433138827823761, 3.000000000000000000, 10.72973591378220704 ) ) ;
#12031 = CARTESIAN_POINT ( 'NONE',  ( -13.50994833511691340, 0.000000000000000000, -1.105736515254444052 ) ) ;
#12032 = ORIENTED_EDGE ( 'NONE', *, *, #8027, .F. ) ;
#12033 = ORIENTED_EDGE ( 'NONE', *, *, #2302, .F. ) ;
#12034 = ORIENTED_EDGE ( 'NONE', *, *, #10686, .T. ) ;
#12035 = DIRECTION ( 'NONE',  ( 0.000000000000000000, 0.000000000000000000, 1.000000000000000000 ) ) ;
#12036 = CARTESIAN_POINT ( 'NONE',  ( -14.87484884897975057, 0.000000000000000000, 1.958311002203303453 ) ) ;
#12037 = DIRECTION ( 'NONE',  ( 1.000000000000000000, 0.000000000000000000, 0.000000000000000000 ) ) ;
#12038 = CARTESIAN_POINT ( 'NONE',  ( 0.7944557581062194895, 0.000000000000000000, -6.703084368289861317 ) ) ;
#12039 = LINE ( 'NONE', #3755, #1779 ) ;
#12040 = EDGE_CURVE ( 'NONE', #8456, #4963, #3190, .T. ) ;
#12041 = PRODUCT_RELATED_PRODUCT_CATEGORY ( 'part', '', ( #12619 ) ) ;
#12042 = CARTESIAN_POINT ( 'NONE',  ( -11.63517940784383775, 3.000000000000000000, -7.494008246337203083 ) ) ;
#12043 = CARTESIAN_POINT ( 'NONE',  ( 0.000000000000000000, 9.000000000000000000, 0.000000000000000000 ) ) ;
#12044 = DIRECTION ( 'NONE',  ( -3.469446951953614189E-15, -1.000000000000000000, 0.000000000000000000 ) ) ;
#12045 = VERTEX_POINT ( 'NONE', #9168 ) ;
#12046 = VERTEX_POINT ( 'NONE', #9022 ) ;
#12047 = VERTEX_POINT ( 'NONE', #10066 ) ;
#12048 = PLANE ( 'NONE',  #1161 ) ;
#12049 = ORIENTED_EDGE ( 'NONE', *, *, #5240, .T. ) ;
#12050 = PLANE ( 'NONE',  #8123 ) ;
#12051 = EDGE_CURVE ( 'NONE', #6704, #11685, #9782, .T. ) ;
#12052 = FACE_OUTER_BOUND ( 'NONE', #5939, .T. ) ;
#12053 = DIRECTION ( 'NONE',  ( 0.000000000000000000, 0.000000000000000000, 1.000000000000000000 ) ) ;
#12054 = EDGE_CURVE ( 'NONE', #8874, #1651, #12218, .T. ) ;
#12055 = CARTESIAN_POINT ( 'NONE',  ( 2.392396671352952087, 9.000000000000000000, 6.311809420990097230 ) ) ;
#12056 = DIRECTION ( 'NONE',  ( 0.000000000000000000, 1.000000000000000000, 0.000000000000000000 ) ) ;
#12057 = CARTESIAN_POINT ( 'NONE',  ( 1.836970198721030181E-16, 1.000000000000000000, 1.500000000000000222 ) ) ;
#12058 = ORIENTED_EDGE ( 'NONE', *, *, #11732, .F. ) ;
#12059 = ADVANCED_FACE ( 'NONE', ( #10131 ), #4902, .F. ) ;
#12060 = CARTESIAN_POINT ( 'NONE',  ( -5.731782959214987372, 3.000000000000000000, -11.46814821560793618 ) ) ;
#12061 = EDGE_CURVE ( 'NONE', #11907, #9840, #3847, .T. ) ;
#12062 = ORIENTED_EDGE ( 'NONE', *, *, #7177, .F. ) ;
#12063 = UNCERTAINTY_MEASURE_WITH_UNIT (LENGTH_MEASURE( 1.000000000000000082E-05 ), #8067, 'distance_accuracy_value', 'NONE');
#12064 = ORIENTED_EDGE ( 'NONE', *, *, #2532, .T. ) ;
#12065 = CARTESIAN_POINT ( 'NONE',  ( 13.11311062740304401, 3.000000000000000000, -1.563624455674628377 ) ) ;
#12066 = VERTEX_POINT ( 'NONE', #12622 ) ;
#12067 = VERTEX_POINT ( 'NONE', #1943 ) ;
#12068 = CARTESIAN_POINT ( 'NONE',  ( 4.898587196589413075E-17, 9.000000000000000000, 0.4000000000000000222 ) ) ;
#12069 =( LENGTH_UNIT ( ) NAMED_UNIT ( * ) SI_UNIT ( .MILLI., .METRE. ) );
#12070 = CARTESIAN_POINT ( 'NONE',  ( -8.222660081691577361, 0.000000000000000000, -5.549999999999999822 ) ) ;
#12071 = EDGE_CURVE ( 'NONE', #6591, #1437, #1490, .T. ) ;
#12072 = CARTESIAN_POINT ( 'NONE',  ( 8.481367827640703183, 0.000000000000000000, 0.5624942419805130100 ) ) ;
#12073 = PLANE ( 'NONE',  #13513 ) ;
#12074 = DIRECTION ( 'NONE',  ( 0.6291930273683257191, 0.000000000000000000, -0.7772490812545752581 ) ) ;
#12075 = CARTESIAN_POINT ( 'NONE',  ( 31.00000000000000000, 0.09999999999999982514, -3.399999999999999911 ) ) ;
#12076 = ORIENTED_EDGE ( 'NONE', *, *, #5186, .T. ) ;
#12077 = LINE ( 'NONE', #783, #286 ) ;
#12078 = EDGE_CURVE ( 'NONE', #12207, #1651, #12677, .T. ) ;
#12079 = ORIENTED_EDGE ( 'NONE', *, *, #4336, .F. ) ;
#12080 = PRODUCT_DEFINITION_SHAPE ( 'NONE', 'NONE',  #13605 ) ;
#12081 = ORIENTED_EDGE ( 'NONE', *, *, #11541, .T. ) ;
#12082 = VERTEX_POINT ( 'NONE', #12555 ) ;
#12083 = DIRECTION ( 'NONE',  ( 0.000000000000000000, 0.000000000000000000, 1.000000000000000000 ) ) ;
#12084 = DIRECTION ( 'NONE',  ( -0.000000000000000000, -1.000000000000000000, -0.000000000000000000 ) ) ;
#12085 = DIRECTION ( 'NONE',  ( 0.000000000000000000, 1.000000000000000000, 0.000000000000000000 ) ) ;
#12086 = EDGE_CURVE ( 'NONE', #5803, #3424, #7382, .T. ) ;
#12087 = CARTESIAN_POINT ( 'NONE',  ( 30.82048254704846713, 3.000000000000000000, -7.998976482636475538 ) ) ;
#12088 = EDGE_CURVE ( 'NONE', #3702, #8770, #13319, .T. ) ;
#12089 = CARTESIAN_POINT ( 'NONE',  ( -5.299649803506882861, 0.000000000000000000, -6.645578376649353913 ) ) ;
#12090 = DIRECTION ( 'NONE',  ( 0.000000000000000000, 0.000000000000000000, -1.000000000000000000 ) ) ;
#12091 = CARTESIAN_POINT ( 'NONE',  ( -8.430890348300632553, 0.000000000000000000, -11.48836750521723538 ) ) ;
#12092 = DIRECTION ( 'NONE',  ( 0.000000000000000000, 0.000000000000000000, 1.000000000000000000 ) ) ;
#12093 = CARTESIAN_POINT ( 'NONE',  ( -7.798201703419555209, 3.000000000000000000, -30.99999999999999289 ) ) ;
#12094 = CARTESIAN_POINT ( 'NONE',  ( 0.5400000000008001733, 3.000000000000000000, 12.07793442604883616 ) ) ;
#12095 = ORIENTED_EDGE ( 'NONE', *, *, #1543, .F. ) ;
#12096 = VERTEX_POINT ( 'NONE', #10413 ) ;
#12097 = CIRCLE ( 'NONE', #10983, 8.500000000000000000 ) ;
#12098 = ORIENTED_EDGE ( 'NONE', *, *, #9541, .F. ) ;
#12099 = FACE_OUTER_BOUND ( 'NONE', #4610, .T. ) ;
#12100 = CARTESIAN_POINT ( 'NONE',  ( 6.506620931068707314, 0.000000000000000000, 10.18979803820051622 ) ) ;
#12101 = EDGE_CURVE ( 'NONE', #284, #4963, #91, .T. ) ;
#12102 = CARTESIAN_POINT ( 'NONE',  ( 0.000000000000000000, 0.000000000000000000, 0.000000000000000000 ) ) ;
#12103 = VECTOR ( 'NONE', #2937, 1000.000000000000000 ) ;
#12104 = LINE ( 'NONE', #9753, #11012 ) ;
#12105 = CARTESIAN_POINT ( 'NONE',  ( 5.053288777954493050, 9.000000000000000000, -4.475128213425755952 ) ) ;
#12106 = AXIS2_PLACEMENT_3D ( 'NONE', #2634, #11394, #6286 ) ;
#12107 = CARTESIAN_POINT ( 'NONE',  ( 12.01285915242476499, 3.000000000000000000, -4.000000001073668265 ) ) ;
#12108 = CARTESIAN_POINT ( 'NONE',  ( -11.48836750521728689, 0.000000000000000000, -8.430890348300561499 ) ) ;
#12109 = CARTESIAN_POINT ( 'NONE',  ( 8.914835885878215294, 0.000000000000000000, 11.11702303352197418 ) ) ;
#12110 = ORIENTED_EDGE ( 'NONE', *, *, #1066, .T. ) ;
#12111 = ORIENTED_EDGE ( 'NONE', *, *, #5313, .F. ) ;
#12112 = VERTEX_POINT ( 'NONE', #10545 ) ;
#12113 = DIRECTION ( 'NONE',  ( 0.000000000000000000, 0.000000000000000000, 1.000000000000000000 ) ) ;
#12114 = CIRCLE ( 'NONE', #8140, 1.500000000000001332 ) ;
#12115 = CIRCLE ( 'NONE', #1552, 14.25000000000000178 ) ;
#12116 = EDGE_CURVE ( 'NONE', #1266, #5996, #2140, .T. ) ;
#12117 = ORIENTED_EDGE ( 'NONE', *, *, #5476, .T. ) ;
#12118 = CARTESIAN_POINT ( 'NONE',  ( 5.733772933379474246, 3.000000000000000000, -13.04554897075799502 ) ) ;
#12119 = CARTESIAN_POINT ( 'NONE',  ( 28.67696780347060681, 35.33135765298362685, 66.33042399990208082 ) ) ;
#12120 = CARTESIAN_POINT ( 'NONE',  ( -1.557181465540760534, 3.000000000000000000, -14.16466328168009703 ) ) ;
#12121 = CARTESIAN_POINT ( 'NONE',  ( -6.057461899949976747, 9.000000000000000000, 5.137313564148215939 ) ) ;
#12122 = DIRECTION ( 'NONE',  ( 1.000000000000000000, 0.000000000000000000, 0.000000000000000000 ) ) ;
#12123 = CIRCLE ( 'NONE', #12354, 3.000000000000000888 ) ;
#12124 = CARTESIAN_POINT ( 'NONE',  ( 12.00000000000001243, 4.999999999999999112, 10.00000000000000178 ) ) ;
#12125 = CIRCLE ( 'NONE', #3751, 0.4000000000000000222 ) ;
#12126 = CARTESIAN_POINT ( 'NONE',  ( -12.98835496148299207, 3.000000000000000000, 0.5501230721524459355 ) ) ;
#12127 = ORIENTED_EDGE ( 'NONE', *, *, #3953, .F. ) ;
#12128 = SURFACE_SIDE_STYLE ('',( #4880 ) ) ;
#12129 = EDGE_LOOP ( 'NONE', ( #11164, #847, #5597, #8652 ) ) ;
#12130 = ORIENTED_EDGE ( 'NONE', *, *, #10550, .T. ) ;
#12131 = LINE ( 'NONE', #9009, #8831 ) ;
#12132 = ADVANCED_FACE ( 'NONE', ( #8199 ), #177, .F. ) ;
#12133 = ORIENTED_EDGE ( 'NONE', *, *, #12851, .T. ) ;
#12134 = AXIS2_PLACEMENT_3D ( 'NONE', #7471, #12849, #5262 ) ;
#12135 = AXIS2_PLACEMENT_3D ( 'NONE', #10449, #10579, #12588 ) ;
#12136 = ORIENTED_EDGE ( 'NONE', *, *, #4287, .T. ) ;
#12137 = AXIS2_PLACEMENT_3D ( 'NONE', #10914, #5671, #9869 ) ;
#12138 = DIRECTION ( 'NONE',  ( 0.000000000000000000, 0.000000000000000000, -1.000000000000000000 ) ) ;
#12139 =( LENGTH_UNIT ( ) NAMED_UNIT ( * ) SI_UNIT ( .MILLI., .METRE. ) );
#12140 = DIRECTION ( 'NONE',  ( 0.000000000000000000, 1.000000000000000000, 0.000000000000000000 ) ) ;
#12141 = FACE_OUTER_BOUND ( 'NONE', #5457, .T. ) ;
#12142 = CARTESIAN_POINT ( 'NONE',  ( -11.52330688609014686, 3.000000000000000000, -6.017756925049552841 ) ) ;
#12143 = DIRECTION ( 'NONE',  ( 0.000000000000000000, 1.000000000000000000, 0.000000000000000000 ) ) ;
#12144 = ORIENTED_EDGE ( 'NONE', *, *, #10056, .T. ) ;
#12145 = DIRECTION ( 'NONE',  ( -0.000000000000000000, -1.000000000000000000, -0.000000000000000000 ) ) ;
#12146 = VECTOR ( 'NONE', #2691, 1000.000000000000000 ) ;
#12147 = ORIENTED_EDGE ( 'NONE', *, *, #11057, .F. ) ;
#12148 = EDGE_LOOP ( 'NONE', ( #9172, #9969, #2855, #10394 ) ) ;
#12149 = DIRECTION ( 'NONE',  ( -0.000000000000000000, -1.000000000000000000, -0.000000000000000000 ) ) ;
#12150 = EDGE_CURVE ( 'NONE', #6731, #1406, #6203, .T. ) ;
#12151 = ORIENTED_EDGE ( 'NONE', *, *, #1115, .F. ) ;
#12152 = CARTESIAN_POINT ( 'NONE',  ( 5.053288777954493050, 9.000000000000000000, -4.475128213425755952 ) ) ;
#12153 = AXIS2_PLACEMENT_3D ( 'NONE', #8566, #1220, #8707 ) ;
#12154 = ADVANCED_FACE ( 'NONE', ( #12434 ), #12926, .F. ) ;
#12155 = DIRECTION ( 'NONE',  ( -0.000000000000000000, -1.000000000000000000, -0.000000000000000000 ) ) ;
#12156 = ADVANCED_FACE ( 'NONE', ( #1106 ), #5301, .T. ) ;
#12157 = VECTOR ( 'NONE', #5269, 1000.000000000000000 ) ;
#12158 = CARTESIAN_POINT ( 'NONE',  ( -8.771102293099080072, 3.000000000000000000, -10.33484986938307770 ) ) ;
#12159 = CARTESIAN_POINT ( 'NONE',  ( 4.286263797015737088E-16, 0.09999999999999982514, 3.500000000000000888 ) ) ;
#12160 = LINE ( 'NONE', #2576, #2642 ) ;
#12161 = ITEM_DEFINED_TRANSFORMATION ( 'NONE', 'NONE', #2110,  #10007 ) ;
#12162 = CARTESIAN_POINT ( 'NONE',  ( -9.573149624528719315, 0.000000000000000000, -8.795158114916407754 ) ) ;
#12163 = CARTESIAN_POINT ( 'NONE',  ( 3.555260608155774271, 0.000000000000000000, 7.720759160088842776 ) ) ;
#12164 = FACE_BOUND ( 'NONE', #12648, .T. ) ;
#12165 = DIRECTION ( 'NONE',  ( 0.000000000000000000, 0.000000000000000000, 1.000000000000000000 ) ) ;
#12166 = DIRECTION ( 'NONE',  ( -0.000000000000000000, -1.000000000000000000, -0.000000000000000000 ) ) ;
#12167 = APPLICATION_CONTEXT ( 'automotive_design' ) ;
#12168 = EDGE_LOOP ( 'NONE', ( #7636, #6632, #1309, #8670 ) ) ;
#12169 = VECTOR ( 'NONE', #223, 1000.000000000000000 ) ;
#12170 = ORIENTED_EDGE ( 'NONE', *, *, #6168, .T. ) ;
#12171 = AXIS2_PLACEMENT_3D ( 'NONE', #2763, #12140, #8885 ) ;
#12172 = AXIS2_PLACEMENT_3D ( 'NONE', #6563, #10762, #1325 ) ;
#12173 = EDGE_CURVE ( 'NONE', #5132, #116, #12499, .T. ) ;
#12174 = ORIENTED_EDGE ( 'NONE', *, *, #12712, .T. ) ;
#12175 = CARTESIAN_POINT ( 'NONE',  ( 5.797378255456016483, 0.000000000000000000, 12.25282671965375592 ) ) ;
#12176 = LINE ( 'NONE', #11887, #13524 ) ;
#12177 = AXIS2_PLACEMENT_3D ( 'NONE', #3355, #343, #4334 ) ;
#12178 = DIRECTION ( 'NONE',  ( 0.000000000000000000, 1.000000000000000000, 0.000000000000000000 ) ) ;
#12179 = VECTOR ( 'NONE', #1974, 1000.000000000000000 ) ;
#12180 = VECTOR ( 'NONE', #411, 1000.000000000000000 ) ;
#12181 = DIRECTION ( 'NONE',  ( -0.000000000000000000, -1.000000000000000000, -0.000000000000000000 ) ) ;
#12182 = LINE ( 'NONE', #2655, #3521 ) ;
#12183 = DIRECTION ( 'NONE',  ( 0.000000000000000000, 0.000000000000000000, -1.000000000000000000 ) ) ;
#12184 = DIRECTION ( 'NONE',  ( 0.000000000000000000, -0.000000000000000000, 1.000000000000000000 ) ) ;
#12185 = CARTESIAN_POINT ( 'NONE',  ( 0.000000000000000000, 9.000000000000000000, 0.000000000000000000 ) ) ;
#12186 = ORIENTED_EDGE ( 'NONE', *, *, #11996, .F. ) ;
#12187 = EDGE_CURVE ( 'NONE', #1383, #13316, #2009, .T. ) ;
#12188 = ORIENTED_EDGE ( 'NONE', *, *, #936, .F. ) ;
#12189 = ORIENTED_EDGE ( 'NONE', *, *, #5934, .T. ) ;
#12190 = AXIS2_PLACEMENT_3D ( 'NONE', #2683, #9480, #6312 ) ;
#12191 = CARTESIAN_POINT ( 'NONE',  ( -2.604399508763951321, 0.000000000000000000, 11.80615107470197422 ) ) ;
#12192 = AXIS2_PLACEMENT_3D ( 'NONE', #4090, #35, #9246 ) ;
#12193 = VERTEX_POINT ( 'NONE', #10483 ) ;
#12194 = DIRECTION ( 'NONE',  ( -0.000000000000000000, -1.000000000000000000, -0.000000000000000000 ) ) ;
#12195 = DIRECTION ( 'NONE',  ( 0.000000000000000000, 0.000000000000000000, 1.000000000000000000 ) ) ;
#12196 = CARTESIAN_POINT ( 'NONE',  ( 12.00000000000002309, 8.000000000000000000, 7.000000000000000888 ) ) ;
#12197 = CARTESIAN_POINT ( 'NONE',  ( 11.90209577080759296, 3.000000000000000000, -8.180229652970856691 ) ) ;
#12198 = DIRECTION ( 'NONE',  ( 1.261435711112880913E-16, 0.000000000000000000, 1.000000000000000000 ) ) ;
#12199 = CIRCLE ( 'NONE', #8004, 12.99999999999977973 ) ;
#12200 = DIRECTION ( 'NONE',  ( 0.000000000000000000, 0.000000000000000000, 1.000000000000000000 ) ) ;
#12201 = CARTESIAN_POINT ( 'NONE',  ( -0.8973464813148227526, 9.000000000000000000, -7.308217849399443189 ) ) ;
#12202 = EDGE_LOOP ( 'NONE', ( #5103, #11468, #7829, #2647 ) ) ;
#12203 = CARTESIAN_POINT ( 'NONE',  ( -5.797378255456022700, 0.000000000000000000, -12.25282671965375592 ) ) ;
#12204 = ORIENTED_EDGE ( 'NONE', *, *, #7450, .F. ) ;
#12205 = VERTEX_POINT ( 'NONE', #4136 ) ;
#12206 = CARTESIAN_POINT ( 'NONE',  ( -2.161962830978702677, 3.000000000000000000, 14.08504230442587435 ) ) ;
#12207 = VERTEX_POINT ( 'NONE', #9437 ) ;
#12208 = CIRCLE ( 'NONE', #539, 8.499999999999996447 ) ;
#12209 = DIRECTION ( 'NONE',  ( 0.000000000000000000, 0.000000000000000000, -1.000000000000000000 ) ) ;
#12210 = AXIS2_PLACEMENT_3D ( 'NONE', #9421, #4052, #10390 ) ;
#12211 = VERTEX_POINT ( 'NONE', #17 ) ;
#12212 = CARTESIAN_POINT ( 'NONE',  ( 3.555260608155775159, 0.000000000000000000, 7.720759160088846329 ) ) ;
#12213 = CARTESIAN_POINT ( 'NONE',  ( -6.017756925049793537, 3.000000000000000000, -11.52330688609026232 ) ) ;
#12214 = CARTESIAN_POINT ( 'NONE',  ( 0.5400000000008007284, 3.000000000000000000, 12.07793442604883793 ) ) ;
#12215 = B_SPLINE_CURVE_WITH_KNOTS ( 'NONE', 3,
 ( #5386, #34, #2290, #473 ),
 .UNSPECIFIED., .F., .F.,
 ( 4, 4 ),
 ( 0.8181806201944104018, 0.8475986972523573693 ),
 .UNSPECIFIED. ) ;
#12216 = DIRECTION ( 'NONE',  ( 0.000000000000000000, 1.000000000000000000, -0.000000000000000000 ) ) ;
#12217 = CARTESIAN_POINT ( 'NONE',  ( -5.526615004551211463, 9.000000000000000000, -4.866191470063547797 ) ) ;
#12218 = LINE ( 'NONE', #1741, #1654 ) ;
#12219 = EDGE_CURVE ( 'NONE', #13401, #12534, #9792, .T. ) ;
#12220 = EDGE_LOOP ( 'NONE', ( #6447, #6295, #10432, #11649 ) ) ;
#12221 = AXIS2_PLACEMENT_3D ( 'NONE', #6568, #7472, #2230 ) ;
#12222 = CARTESIAN_POINT ( 'NONE',  ( 0.000000000000000000, 0.09999999999999982514, 0.000000000000000000 ) ) ;
#12223 = ORIENTED_EDGE ( 'NONE', *, *, #1041, .F. ) ;
#12224 = ORIENTED_EDGE ( 'NONE', *, *, #10323, .T. ) ;
#12225 = CARTESIAN_POINT ( 'NONE',  ( -0.7702044561450404059, 3.000000000000000000, 12.79759916868914793 ) ) ;
#12226 = B_SPLINE_CURVE_WITH_KNOTS ( 'NONE', 3,
 ( #12191, #1715, #673, #4868 ),
 .UNSPECIFIED., .F., .F.,
 ( 4, 4 ),
 ( 0.1547128134717859205, 1.000000000000000000 ),
 .UNSPECIFIED. ) ;
#12227 = VERTEX_POINT ( 'NONE', #8529 ) ;
#12228 = DIRECTION ( 'NONE',  ( -0.000000000000000000, -1.000000000000000000, -0.000000000000000000 ) ) ;
#12229 = AXIS2_PLACEMENT_3D ( 'NONE', #1725, #9905, #5913 ) ;
#12230 = CARTESIAN_POINT ( 'NONE',  ( 12.08646469655232636, 0.000000000000000000, -8.883544964652022813 ) ) ;
#12231 = DIRECTION ( 'NONE',  ( 0.000000000000000000, 0.000000000000000000, 1.000000000000000000 ) ) ;
#12232 = CARTESIAN_POINT ( 'NONE',  ( -13.49999999999999645, 0.000000000000000000, -5.549999999999999822 ) ) ;
#12233 = DIRECTION ( 'NONE',  ( -0.000000000000000000, -1.000000000000000000, -0.000000000000000000 ) ) ;
#12234 = ITEM_DEFINED_TRANSFORMATION ( 'NONE', 'NONE', #9378,  #10007 ) ;
#12235 = DIRECTION ( 'NONE',  ( 0.000000000000000000, 1.000000000000000000, 0.000000000000000000 ) ) ;
#12236 = ADVANCED_FACE ( 'NONE', ( #409 ), #6609, .T. ) ;
#12237 = DIRECTION ( 'NONE',  ( -0.000000000000000000, -1.000000000000000000, -0.000000000000000000 ) ) ;
#12238 = FACE_BOUND ( 'NONE', #13572, .T. ) ;
#12239 = ADVANCED_FACE ( 'NONE', ( #217 ), #2476, .T. ) ;
#12240 = CARTESIAN_POINT ( 'NONE',  ( 11.48836750521724070, 3.000000000000000000, -8.430890348300621895 ) ) ;
#12241 = DIRECTION ( 'NONE',  ( 0.000000000000000000, 1.000000000000000000, 0.000000000000000000 ) ) ;
#12242 = ORIENTED_EDGE ( 'NONE', *, *, #2172, .T. ) ;
#12243 = STYLED_ITEM ( 'NONE', ( #1168 ), #3921 ) ;
#12244 = ADVANCED_FACE ( 'NONE', ( #7707 ), #10806, .T. ) ;
#12245 = EDGE_LOOP ( 'NONE', ( #2223, #5456, #1386, #11979 ) ) ;
#12246 = ADVANCED_FACE ( 'NONE', ( #9579 ), #2135, .F. ) ;
#12247 = ORIENTED_EDGE ( 'NONE', *, *, #10238, .T. ) ;
#12248 = ORIENTED_EDGE ( 'NONE', *, *, #7501, .F. ) ;
#12249 = LINE ( 'NONE', #1700, #8854 ) ;
#12250 = LINE ( 'NONE', #870, #10442 ) ;
#12251 = B_SPLINE_SURFACE_WITH_KNOTS ( 'NONE', 3, 1, ( 
 ( #1021, #9415 ),
 ( #12282, #11096 ),
 ( #1735, #2822 ),
 ( #4244, #10059 ) ),
 .UNSPECIFIED., .F., .F., .F.,
 ( 4, 4 ),
 ( 2, 2 ),
 ( 0.000000000000000000, 0.8452273900860258760 ),
 ( 0.000000000000000000, 1.000000000000000000 ),
 .UNSPECIFIED. ) ;
#12252 = AXIS2_PLACEMENT_3D ( 'NONE', #3846, #8047, #10043 ) ;
#12253 = DIRECTION ( 'NONE',  ( -0.000000000000000000, -1.000000000000000000, -0.000000000000000000 ) ) ;
#12254 = EDGE_CURVE ( 'NONE', #3774, #2677, #5641, .T. ) ;
#12255 = CARTESIAN_POINT ( 'NONE',  ( -5.733772933379540859, 0.000000000000000000, -13.04554897075796660 ) ) ;
#12256 = DIRECTION ( 'NONE',  ( 0.3802634127332067404, -0.000000000000000000, 0.9248782281665489657 ) ) ;
#12257 = DIRECTION ( 'NONE',  ( -0.000000000000000000, -1.000000000000000000, -0.000000000000000000 ) ) ;
#12258 = FACE_OUTER_BOUND ( 'NONE', #9728, .T. ) ;
#12259 = LINE ( 'NONE', #876, #7742 ) ;
#12260 = ORIENTED_EDGE ( 'NONE', *, *, #4580, .F. ) ;
#12261 = EDGE_CURVE ( 'NONE', #4567, #3774, #836, .T. ) ;
#12262 = ORIENTED_EDGE ( 'NONE', *, *, #10108, .T. ) ;
#12263 = ORIENTED_EDGE ( 'NONE', *, *, #13235, .F. ) ;
#12264 = DIRECTION ( 'NONE',  ( 1.000000000000000000, 0.000000000000000000, -3.061616997868383141E-16 ) ) ;
#12265 = VERTEX_POINT ( 'NONE', #8733 ) ;
#12266 = DIRECTION ( 'NONE',  ( 0.000000000000000000, 1.000000000000000000, -0.000000000000000000 ) ) ;
#12267 = DIRECTION ( 'NONE',  ( 1.000000000000000000, 0.000000000000000000, 0.000000000000000000 ) ) ;
#12268 = EDGE_CURVE ( 'NONE', #8454, #7299, #12889, .T. ) ;
#12269 = CARTESIAN_POINT ( 'NONE',  ( 0.000000000000000000, 0.000000000000000000, 0.000000000000000000 ) ) ;
#12270 = LINE ( 'NONE', #10046, #3091 ) ;
#12271 = ADVANCED_FACE ( 'NONE', ( #11646 ), #4607, .T. ) ;
#12272 = CARTESIAN_POINT ( 'NONE',  ( 45.60964950616533287, 0.000000000000000000, -14.50984893380129392 ) ) ;
#12273 = DIRECTION ( 'NONE',  ( 0.000000000000000000, 0.000000000000000000, 1.000000000000000000 ) ) ;
#12274 = CARTESIAN_POINT ( 'NONE',  ( -1.604252589105052307, 0.000000000000000000, -8.347237484961700815 ) ) ;
#12275 = ORIENTED_EDGE ( 'NONE', *, *, #5373, .F. ) ;
#12276 = CYLINDRICAL_SURFACE ( 'NONE', #3142, 8.499999999999998224 ) ;
#12277 = EDGE_CURVE ( 'NONE', #7144, #13474, #12020, .T. ) ;
#12278 = ORIENTED_EDGE ( 'NONE', *, *, #6620, .T. ) ;
#12279 = ORIENTED_EDGE ( 'NONE', *, *, #7911, .F. ) ;
#12280 = CARTESIAN_POINT ( 'NONE',  ( 28.56494132578241008, 3.000000000000000000, -0.9541491613812155270 ) ) ;
#12281 = ORIENTED_EDGE ( 'NONE', *, *, #6599, .F. ) ;
#12282 = CARTESIAN_POINT ( 'NONE',  ( -11.14709020439930676, 3.000000000000000000, -7.712570079660886257 ) ) ;
#12283 = ORIENTED_EDGE ( 'NONE', *, *, #5650, .F. ) ;
#12284 = DIRECTION ( 'NONE',  ( 0.000000000000000000, 1.000000000000000000, 0.000000000000000000 ) ) ;
#12285 = AXIS2_PLACEMENT_3D ( 'NONE', #3650, #2616, #11023 ) ;
#12286 = CARTESIAN_POINT ( 'NONE',  ( -7.712570079660889810, 0.000000000000000000, 11.14709020439930320 ) ) ;
#12287 = DIRECTION ( 'NONE',  ( 0.000000000000000000, 1.000000000000000000, 0.000000000000000000 ) ) ;
#12288 = CARTESIAN_POINT ( 'NONE',  ( 0.000000000000000000, 9.000000000000000000, 0.000000000000000000 ) ) ;
#12289 = CARTESIAN_POINT ( 'NONE',  ( 9.379342464487701037, 0.000000000000000000, -10.98198414889939301 ) ) ;
#12290 = CARTESIAN_POINT ( 'NONE',  ( 0.000000000000000000, 3.000000000000000000, 0.000000000000000000 ) ) ;
#12291 = ORIENTED_EDGE ( 'NONE', *, *, #7133, .T. ) ;
#12292 = DIRECTION ( 'NONE',  ( 0.000000000000000000, 1.000000000000000000, -0.000000000000000000 ) ) ;
#12293 = ORIENTED_EDGE ( 'NONE', *, *, #9690, .T. ) ;
#12294 = ORIENTED_EDGE ( 'NONE', *, *, #3387, .F. ) ;
#12295 = DIRECTION ( 'NONE',  ( -1.000000000000000000, 3.469446951953610639E-15, 2.602085213965210149E-16 ) ) ;
#12296 = ORIENTED_EDGE ( 'NONE', *, *, #7504, .F. ) ;
#12297 = ADVANCED_FACE ( 'NONE', ( #6402 ), #11940, .F. ) ;
#12298 = CARTESIAN_POINT ( 'NONE',  ( 8.914835885878279242, 3.000000000000000000, 11.11702303352191734 ) ) ;
#12299 = CARTESIAN_POINT ( 'NONE',  ( 10.33484986938308481, 3.000000000000000000, -8.771102293099065861 ) ) ;
#12300 = LINE ( 'NONE', #3730, #9509 ) ;
#12301 = CARTESIAN_POINT ( 'NONE',  ( 0.000000000000000000, 14.00000000000000178, 0.000000000000000000 ) ) ;
#12302 = CARTESIAN_POINT ( 'NONE',  ( 12.00000000000001243, 5.250000000000000000, -3.122502256758250009E-15 ) ) ;
#12303 = DIRECTION ( 'NONE',  ( 0.000000000000000000, 0.000000000000000000, 1.000000000000000000 ) ) ;
#12304 = CYLINDRICAL_SURFACE ( 'NONE', #4617, 0.7499999999999997780 ) ;
#12305 = LINE ( 'NONE', #6777, #8801 ) ;
#12306 = DIRECTION ( 'NONE',  ( 1.000000000000000000, 0.000000000000000000, -0.000000000000000000 ) ) ;
#12307 = DIRECTION ( 'NONE',  ( 0.000000000000000000, 0.000000000000000000, -1.000000000000000000 ) ) ;
#12308 = ORIENTED_EDGE ( 'NONE', *, *, #12334, .F. ) ;
#12309 = ORIENTED_EDGE ( 'NONE', *, *, #3952, .F. ) ;
#12310 = B_SPLINE_CURVE_WITH_KNOTS ( 'NONE', 3,
 ( #1104, #216, #4405, #5572 ),
 .UNSPECIFIED., .F., .F.,
 ( 4, 4 ),
 ( 0.000000000000000000, 0.8452273900860258760 ),
 .UNSPECIFIED. ) ;
#12311 = VERTEX_POINT ( 'NONE', #3295 ) ;
#12312 = ADVANCED_FACE ( 'NONE', ( #7508 ), #2345, .T. ) ;
#12313 = VERTEX_POINT ( 'NONE', #5573 ) ;
#12314 = CARTESIAN_POINT ( 'NONE',  ( 31.00000000000000000, 3.000000000000000000, -4.000000001073670930 ) ) ;
#12315 = EDGE_CURVE ( 'NONE', #10298, #12927, #2979, .T. ) ;
#12316 = CARTESIAN_POINT ( 'NONE',  ( 12.00000000000001776, 8.000000000000000000, -6.999999999999999112 ) ) ;
#12317 = CIRCLE ( 'NONE', #6440, 1.499999999999999556 ) ;
#12318 = CARTESIAN_POINT ( 'NONE',  ( 19.65244806805498357, 3.000000000000000000, -6.000000000000000000 ) ) ;
#12319 = EDGE_CURVE ( 'NONE', #7860, #288, #11568, .T. ) ;
#12320 = CARTESIAN_POINT ( 'NONE',  ( 12.57851281883977457, 0.000000000000000000, 3.283445639306028063 ) ) ;
#12321 = CARTESIAN_POINT ( 'NONE',  ( 5.958322434183388694, 0.000000000000000000, -6.062045345451230638 ) ) ;
#12322 = AXIS2_PLACEMENT_3D ( 'NONE', #4746, #2400, #8933 ) ;
#12323 = DIRECTION ( 'NONE',  ( 0.000000000000000000, 1.000000000000000000, 0.000000000000000000 ) ) ;
#12324 = CARTESIAN_POINT ( 'NONE',  ( 6.736042615721505200, 0.000000000000000000, 5.184180733653466433 ) ) ;
#12325 = VERTEX_POINT ( 'NONE', #4957 ) ;
#12326 = CARTESIAN_POINT ( 'NONE',  ( -7.751044794789887504, 0.000000000000000000, 1.733822342365972879 ) ) ;
#12327 = CARTESIAN_POINT ( 'NONE',  ( 0.000000000000000000, 9.000000000000000000, 0.000000000000000000 ) ) ;
#12328 = ADVANCED_FACE ( 'NONE', ( #1582 ), #8940, .F. ) ;
#12329 = VERTEX_POINT ( 'NONE', #9154 ) ;
#12330 = AXIS2_PLACEMENT_3D ( 'NONE', #7624, #330, #2707 ) ;
#12331 = CARTESIAN_POINT ( 'NONE',  ( 31.00000000000000000, 2.900000000000000355, -1.500000000000003997 ) ) ;
#12332 = EDGE_CURVE ( 'NONE', #11354, #12419, #8868, .T. ) ;
#12333 = DIRECTION ( 'NONE',  ( 9.992007221626408864E-16, 0.000000000000000000, 1.000000000000000000 ) ) ;
#12334 = EDGE_CURVE ( 'NONE', #833, #7638, #6803, .T. ) ;
#12335 = DIRECTION ( 'NONE',  ( -0.7772490812545754801, 0.000000000000000000, -0.6291930273683253860 ) ) ;
#12336 = DIRECTION ( 'NONE',  ( -1.000000000000000000, -0.000000000000000000, -1.927470528863118802E-16 ) ) ;
#12337 = LINE ( 'NONE', #12731, #10443 ) ;
#12338 = CARTESIAN_POINT ( 'NONE',  ( -18.21140389626389222, 3.000000000000000000, 12.49772878833446299 ) ) ;
#12339 = FACE_OUTER_BOUND ( 'NONE', #3060, .T. ) ;
#12340 = ORIENTED_EDGE ( 'NONE', *, *, #7660, .F. ) ;
#12341 = FACE_OUTER_BOUND ( 'NONE', #5055, .T. ) ;
#12342 = CIRCLE ( 'NONE', #239, 4.000000000000000000 ) ;
#12343 = ORIENTED_EDGE ( 'NONE', *, *, #1102, .T. ) ;
#12344 = AXIS2_PLACEMENT_3D ( 'NONE', #8266, #7036, #3032 ) ;
#12345 = PRODUCT_DEFINITION_CONTEXT ( 'detailed design', #7231, 'design' ) ;
#12346 = VERTEX_POINT ( 'NONE', #2751 ) ;
#12347 = CARTESIAN_POINT ( 'NONE',  ( 6.217402469309262436, 3.000000000000000000, -13.03533457366732939 ) ) ;
#12348 = EDGE_CURVE ( 'NONE', #8060, #7270, #12370, .T. ) ;
#12349 = EDGE_CURVE ( 'NONE', #2149, #2448, #11687, .T. ) ;
#12350 = VERTEX_POINT ( 'NONE', #12057 ) ;
#12351 = VERTEX_POINT ( 'NONE', #6743 ) ;
#12352 = CYLINDRICAL_SURFACE ( 'NONE', #10837, 14.25000000000000178 ) ;
#12353 =( NAMED_UNIT ( * ) SI_UNIT ( $, .STERADIAN. ) SOLID_ANGLE_UNIT ( ) );
#12354 = AXIS2_PLACEMENT_3D ( 'NONE', #1785, #10257, #552 ) ;
#12355 = CARTESIAN_POINT ( 'NONE',  ( -1.133238802859761973, 0.000000000000000000, -14.39763212228013067 ) ) ;
#12356 = DIRECTION ( 'NONE',  ( 0.000000000000000000, 0.000000000000000000, 1.000000000000000000 ) ) ;
#12357 = CIRCLE ( 'NONE', #12992, 2.999999999999999112 ) ;
#12358 = DIRECTION ( 'NONE',  ( -0.000000000000000000, -1.000000000000000000, -0.000000000000000000 ) ) ;
#12359 = DIRECTION ( 'NONE',  ( 1.000000000000000000, 0.000000000000000000, 0.000000000000000000 ) ) ;
#12360 = PLANE ( 'NONE',  #3399 ) ;
#12361 = ORIENTED_EDGE ( 'NONE', *, *, #7047, .F. ) ;
#12362 = CARTESIAN_POINT ( 'NONE',  ( -14.82803603298502360, 0.000000000000000000, -2.264806262022826644 ) ) ;
#12363 = VERTEX_POINT ( 'NONE', #10947 ) ;
#12364 = ORIENTED_EDGE ( 'NONE', *, *, #7078, .F. ) ;
#12365 = LINE ( 'NONE', #8206, #2245 ) ;
#12366 = ADVANCED_FACE ( 'NONE', ( #1512 ), #5701, .T. ) ;
#12367 = VECTOR ( 'NONE', #2122, 1000.000000000000000 ) ;
#12368 = ADVANCED_FACE ( 'NONE', ( #5776 ), #4753, .T. ) ;
#12369 = ORIENTED_EDGE ( 'NONE', *, *, #12656, .T. ) ;
#12370 = B_SPLINE_CURVE_WITH_KNOTS ( 'NONE', 3,
 ( #13153, #2549, #6958, #2607 ),
 .UNSPECIFIED., .F., .F.,
 ( 4, 4 ),
 ( 0.000000000000000000, 0.8452273900860258760 ),
 .UNSPECIFIED. ) ;
#12371 = CARTESIAN_POINT ( 'NONE',  ( -20.74285254778206067, 0.000000000000000000, 14.10762559394868099 ) ) ;
#12372 = CARTESIAN_POINT ( 'NONE',  ( 9.593885948927676210, 3.000000000000000000, -8.504652361247169168 ) ) ;
#12373 = DIRECTION ( 'NONE',  ( -0.000000000000000000, -1.000000000000000000, -0.000000000000000000 ) ) ;
#12374 = CARTESIAN_POINT ( 'NONE',  ( 13.27898586450067420, 3.000000000000000000, 5.170206418547648397 ) ) ;
#12375 = DIRECTION ( 'NONE',  ( -0.000000000000000000, -1.000000000000000000, -0.000000000000000000 ) ) ;
#12376 = DIRECTION ( 'NONE',  ( 0.000000000000000000, 1.000000000000000000, -0.000000000000000000 ) ) ;
#12377 = CIRCLE ( 'NONE', #6409, 8.500000000000000000 ) ;
#12378 = CARTESIAN_POINT ( 'NONE',  ( -7.077546079049271910, 3.000000000000000000, -10.67828022838850544 ) ) ;
#12379 = CARTESIAN_POINT ( 'NONE',  ( 12.08646469655232636, 0.000000000000000000, -8.883544964652022813 ) ) ;
#12380 = CARTESIAN_POINT ( 'NONE',  ( -6.558450276537426404, 9.000000000000000000, -1.596630818375423866 ) ) ;
#12381 = CARTESIAN_POINT ( 'NONE',  ( 2.999999999999997335, 2.000000000000000000, -7.000000000000001776 ) ) ;
#12382 = ORIENTED_EDGE ( 'NONE', *, *, #13345, .T. ) ;
#12383 = ORIENTED_EDGE ( 'NONE', *, *, #5650, .T. ) ;
#12384 = EDGE_LOOP ( 'NONE', ( #10198, #11320, #9222, #3262 ) ) ;
#12385 = CIRCLE ( 'NONE', #8174, 3.999999999999998224 ) ;
#12386 = AXIS2_PLACEMENT_3D ( 'NONE', #12338, #13426, #8052 ) ;
#12387 = ORIENTED_EDGE ( 'NONE', *, *, #4817, .F. ) ;
#12388 = DIRECTION ( 'NONE',  ( -0.000000000000000000, -1.000000000000000000, -0.000000000000000000 ) ) ;
#12389 =( LENGTH_UNIT ( ) NAMED_UNIT ( * ) SI_UNIT ( .MILLI., .METRE. ) );
#12390 = CARTESIAN_POINT ( 'NONE',  ( 0.5400000000008001733, 0.000000000000000000, 12.07793442604883616 ) ) ;
#12391 = DIRECTION ( 'NONE',  ( 0.000000000000000000, 0.000000000000000000, 1.000000000000000000 ) ) ;
#12392 = CARTESIAN_POINT ( 'NONE',  ( 6.506507307819716424, 0.000000000000000000, -10.18987059060247269 ) ) ;
#12393 = VECTOR ( 'NONE', #8005, 1000.000000000000000 ) ;
#12394 = AXIS2_PLACEMENT_3D ( 'NONE', #2778, #4635, #6985 ) ;
#12395 = CIRCLE ( 'NONE', #10176, 1.000000000000000888 ) ;
#12396 = CARTESIAN_POINT ( 'NONE',  ( -13.52637830886139092, 3.000000000000000000, 2.928250210355532790 ) ) ;
#12397 = EDGE_CURVE ( 'NONE', #43, #9336, #687, .T. ) ;
#12398 = ORIENTED_EDGE ( 'NONE', *, *, #11874, .T. ) ;
#12399 = B_SPLINE_SURFACE_WITH_KNOTS ( 'NONE', 3, 1, ( 
 ( #904, #9096 ),
 ( #8129, #2897 ),
 ( #9377, #13312 ),
 ( #5176, #13515 ) ),
 .UNSPECIFIED., .F., .F., .F.,
 ( 4, 4 ),
 ( 2, 2 ),
 ( 0.000000000000000000, 0.8724294488011768989 ),
 ( 0.000000000000000000, 1.000000000000000000 ),
 .UNSPECIFIED. ) ;
#12400 = FACE_OUTER_BOUND ( 'NONE', #1306, .T. ) ;
#12401 = CARTESIAN_POINT ( 'NONE',  ( -4.821006024661084410, 3.000000000000000000, -13.61374091949017640 ) ) ;
#12402 = B_SPLINE_CURVE_WITH_KNOTS ( 'NONE', 3,
 ( #11699, #11906, #8784, #3281 ),
 .UNSPECIFIED., .F., .F.,
 ( 4, 4 ),
 ( 0.000000000000000000, 0.8452273900860258760 ),
 .UNSPECIFIED. ) ;
#12403 = ORIENTED_EDGE ( 'NONE', *, *, #7812, .T. ) ;
#12404 = AXIS2_PLACEMENT_3D ( 'NONE', #1363, #5561, #10936 ) ;
#12405 = CIRCLE ( 'NONE', #1612, 1.500000000000001332 ) ;
#12406 = AXIS2_PLACEMENT_3D ( 'NONE', #7982, #8942, #9003 ) ;
#12407 = DIRECTION ( 'NONE',  ( 0.000000000000000000, 0.000000000000000000, 1.000000000000000000 ) ) ;
#12408 = DIRECTION ( 'NONE',  ( 1.000000000000000000, 0.000000000000000000, -9.992007221626408864E-16 ) ) ;
#12409 = CARTESIAN_POINT ( 'NONE',  ( -13.33788847341978645, 0.000000000000000000, -2.414978278956336322 ) ) ;
#12410 = CARTESIAN_POINT ( 'NONE',  ( 2.161962830978694683, 3.000000000000000000, -14.08504230442587790 ) ) ;
#12411 = DIRECTION ( 'NONE',  ( 0.000000000000000000, 0.000000000000000000, 1.000000000000000000 ) ) ;
#12412 = EDGE_CURVE ( 'NONE', #4927, #11338, #11341, .T. ) ;
#12413 = LINE ( 'NONE', #9074, #6423 ) ;
#12414 = LINE ( 'NONE', #5223, #8900 ) ;
#12415 = EDGE_CURVE ( 'NONE', #13469, #6080, #13094, .T. ) ;
#12416 = VECTOR ( 'NONE', #12388, 1000.000000000000000 ) ;
#12417 = CARTESIAN_POINT ( 'NONE',  ( -0.5398653231797316820, 0.000000000000000000, 12.07794044664754018 ) ) ;
#12418 = VECTOR ( 'NONE', #4638, 1000.000000000000000 ) ;
#12419 = VERTEX_POINT ( 'NONE', #12126 ) ;
#12420 = VERTEX_POINT ( 'NONE', #8870 ) ;
#12421 = ADVANCED_FACE ( 'NONE', ( #3852 ), #4813, .T. ) ;
#12422 = ORIENTED_EDGE ( 'NONE', *, *, #9036, .F. ) ;
#12423 = CARTESIAN_POINT ( 'NONE',  ( 2.453448243599948952, 2.900000000000000355, 2.353846153846153921 ) ) ;
#12424 = ADVANCED_FACE ( 'NONE', ( #8054 ), #62, .T. ) ;
#12425 = ORIENTED_EDGE ( 'NONE', *, *, #31, .F. ) ;
#12426 = DIRECTION ( 'NONE',  ( -0.000000000000000000, -1.000000000000000000, 0.000000000000000000 ) ) ;
#12427 = CIRCLE ( 'NONE', #4044, 2.999999999999992450 ) ;
#12428 = SHAPE_REPRESENTATION_RELATIONSHIP ( 'NONE' , 'NONE' ,  #8539, #13452 ) ;
#12429 = CARTESIAN_POINT ( 'NONE',  ( -6.970598036433426792, 0.000000000000000000, -10.97318381393771780 ) ) ;
#12430 = FACE_OUTER_BOUND ( 'NONE', #3795, .T. ) ;
#12431 = DIRECTION ( 'NONE',  ( 0.000000000000000000, 0.000000000000000000, 1.000000000000000000 ) ) ;
#12432 = EDGE_CURVE ( 'NONE', #9336, #8880, #4302, .T. ) ;
#12433 = FACE_OUTER_BOUND ( 'NONE', #2625, .T. ) ;
#12434 = FACE_OUTER_BOUND ( 'NONE', #2742, .T. ) ;
#12435 = ORIENTED_EDGE ( 'NONE', *, *, #2150, .T. ) ;
#12436 = CYLINDRICAL_SURFACE ( 'NONE', #6017, 3.000000000000000888 ) ;
#12437 = ORIENTED_EDGE ( 'NONE', *, *, #5313, .T. ) ;
#12438 = AXIS2_PLACEMENT_3D ( 'NONE', #12043, #5896, #8922 ) ;
#12439 = EDGE_LOOP ( 'NONE', ( #11604, #3707 ) ) ;
#12440 = VECTOR ( 'NONE', #1354, 1000.000000000000000 ) ;
#12441 = CARTESIAN_POINT ( 'NONE',  ( 2.394769219159762041, 9.000000000000000000, -6.310909632292713844 ) ) ;
#12442 = ORIENTED_EDGE ( 'NONE', *, *, #7752, .F. ) ;
#12443 = CARTESIAN_POINT ( 'NONE',  ( 2.830255545554135832, 3.000000000000000000, -12.68816982652952596 ) ) ;
#12444 = DIRECTION ( 'NONE',  ( -0.000000000000000000, -1.000000000000000000, -0.000000000000000000 ) ) ;
#12445 = CARTESIAN_POINT ( 'NONE',  ( -12.08646469655240097, 0.000000000000000000, -8.883544964651921561 ) ) ;
#12446 = DIRECTION ( 'NONE',  ( -0.000000000000000000, -1.000000000000000000, -0.000000000000000000 ) ) ;
#12447 = DIRECTION ( 'NONE',  ( -0.000000000000000000, -1.000000000000000000, -0.000000000000000000 ) ) ;
#12448 = ITEM_DEFINED_TRANSFORMATION ( 'NONE', 'NONE', #5406,  #10007 ) ;
#12449 = CARTESIAN_POINT ( 'NONE',  ( 30.79786191028635400, 3.000000000000000000, -6.999232361977355765 ) ) ;
#12450 = VECTOR ( 'NONE', #6223, 1000.000000000000000 ) ;
#12451 = EDGE_CURVE ( 'NONE', #6481, #8350, #522, .T. ) ;
#12452 = CARTESIAN_POINT ( 'NONE',  ( -7.500000000000000000, 0.000000000000000000, -1.500000000000000666 ) ) ;
#12453 = LINE ( 'NONE', #6096, #3540 ) ;
#12454 = ADVANCED_FACE ( 'NONE', ( #12339 ), #9833, .F. ) ;
#12455 = VECTOR ( 'NONE', #167, 1000.000000000000000 ) ;
#12456 = ORIENTED_EDGE ( 'NONE', *, *, #12412, .T. ) ;
#12457 = LINE ( 'NONE', #6358, #11055 ) ;
#12458 = EDGE_LOOP ( 'NONE', ( #3118, #8780, #11172, #9664 ) ) ;
#12459 = ORIENTED_EDGE ( 'NONE', *, *, #9844, .F. ) ;
#12460 = ADVANCED_FACE ( 'NONE', ( #6319 ), #4517, .T. ) ;
#12461 = VERTEX_POINT ( 'NONE', #3021 ) ;
#12462 = AXIS2_PLACEMENT_3D ( 'NONE', #3184, #4417, #8541 ) ;
#12463 = AXIS2_PLACEMENT_3D ( 'NONE', #11767, #9487, #143 ) ;
#12464 = ORIENTED_EDGE ( 'NONE', *, *, #8643, .T. ) ;
#12465 = LINE ( 'NONE', #12524, #12416 ) ;
#12466 = DIRECTION ( 'NONE',  ( 0.5795187626277481518, 0.000000000000000000, 0.8149588969772670888 ) ) ;
#12467 = CARTESIAN_POINT ( 'NONE',  ( 10.00000000000001421, 6.000000000000007105, -2.602085213965208275E-15 ) ) ;
#12468 = FACE_OUTER_BOUND ( 'NONE', #7965, .T. ) ;
#12469 = CARTESIAN_POINT ( 'NONE',  ( 0.000000000000000000, 3.000000000000000000, 0.000000000000000000 ) ) ;
#12470 = CARTESIAN_POINT ( 'NONE',  ( 0.000000000000000000, 0.000000000000000000, 0.000000000000000000 ) ) ;
#12471 = DIRECTION ( 'NONE',  ( 0.000000000000000000, 1.000000000000000000, 0.000000000000000000 ) ) ;
#12472 = EDGE_LOOP ( 'NONE', ( #3280, #10851, #11134, #4790 ) ) ;
#12473 = CARTESIAN_POINT ( 'NONE',  ( -8.369528376005813897, 0.000000000000000000, 1.483574994138652903 ) ) ;
#12474 = DIRECTION ( 'NONE',  ( 0.000000000000000000, 1.000000000000000000, 0.000000000000000000 ) ) ;
#12475 = ORIENTED_EDGE ( 'NONE', *, *, #10121, .T. ) ;
#12476 = PRODUCT_DEFINITION_FORMATION_WITH_SPECIFIED_SOURCE ( 'ANY', '', #9617, .NOT_KNOWN. ) ;
#12477 = EDGE_CURVE ( 'NONE', #3444, #10793, #8552, .T. ) ;
#12478 = CARTESIAN_POINT ( 'NONE',  ( 11.46847481510586775, 0.000000000000000000, 5.708888906988908829 ) ) ;
#12479 = PRODUCT_CONTEXT ( 'NONE', #10114, 'mechanical' ) ;
#12480 = CARTESIAN_POINT ( 'NONE',  ( -13.33788847341978645, 3.000000000000000000, -2.414978278956336322 ) ) ;
#12481 = CARTESIAN_POINT ( 'NONE',  ( 2.161962830978782613, 3.000000000000000000, 14.08504230442586369 ) ) ;
#12482 = FACE_OUTER_BOUND ( 'NONE', #5127, .T. ) ;
#12483 = LINE ( 'NONE', #11573, #1007 ) ;
#12484 = CARTESIAN_POINT ( 'NONE',  ( 2.161962830978694683, 0.000000000000000000, -14.08504230442587790 ) ) ;
#12485 = ORIENTED_EDGE ( 'NONE', *, *, #13235, .T. ) ;
#12486 = ORIENTED_EDGE ( 'NONE', *, *, #8352, .F. ) ;
#12487 = CARTESIAN_POINT ( 'NONE',  ( 31.00000000000000000, 3.000000000000000000, -3.399999999999999911 ) ) ;
#12488 = ORIENTED_EDGE ( 'NONE', *, *, #12150, .F. ) ;
#12489 = EDGE_CURVE ( 'NONE', #12572, #5689, #12414, .T. ) ;
#12490 = EDGE_CURVE ( 'NONE', #1998, #11792, #9045, .T. ) ;
#12491 = CARTESIAN_POINT ( 'NONE',  ( 0.000000000000000000, 9.000000000000000000, -0.4000000000000000222 ) ) ;
#12492 =( LENGTH_UNIT ( ) NAMED_UNIT ( * ) SI_UNIT ( .MILLI., .METRE. ) );
#12493 = LINE ( 'NONE', #2896, #4910 ) ;
#12494 = CARTESIAN_POINT ( 'NONE',  ( 26.30958424017656938, 3.000000000000000000, -1.399999999999999911 ) ) ;
#12495 = ADVANCED_FACE ( 'NONE', ( #10260 ), #5323, .F. ) ;
#12496 = CARTESIAN_POINT ( 'NONE',  ( -8.795158114916672432, 0.000000000000000000, -9.573149624528774382 ) ) ;
#12497 = EDGE_CURVE ( 'NONE', #13098, #4042, #2318, .T. ) ;
#12498 = CARTESIAN_POINT ( 'NONE',  ( 10.97318381393774089, 0.000000000000000000, -6.970598036433387712 ) ) ;
#12499 = LINE ( 'NONE', #7244, #3199 ) ;
#12500 = VERTEX_POINT ( 'NONE', #1086 ) ;
#12501 = LINE ( 'NONE', #5182, #731 ) ;
#12502 = ORIENTED_EDGE ( 'NONE', *, *, #11206, .F. ) ;
#12503 = EDGE_LOOP ( 'NONE', ( #1965, #12596, #10067, #11499 ) ) ;
#12504 = CARTESIAN_POINT ( 'NONE',  ( -11.80612203322752585, 3.000000000000000000, 2.604531154829235362 ) ) ;
#12505 = ORIENTED_EDGE ( 'NONE', *, *, #8085, .F. ) ;
#12506 = EDGE_CURVE ( 'NONE', #7435, #5535, #5020, .T. ) ;
#12507 = CARTESIAN_POINT ( 'NONE',  ( 3.000000000000001776, 2.000000000000000000, 7.000000000000000000 ) ) ;
#12508 = PRESENTATION_STYLE_ASSIGNMENT (( #715 ) ) ;
#12509 = CARTESIAN_POINT ( 'NONE',  ( 2.623034112301249721, 9.000000000000000000, -7.496701717520498853 ) ) ;
#12510 = DIRECTION ( 'NONE',  ( 0.000000000000000000, 0.000000000000000000, -1.000000000000000000 ) ) ;
#12511 = CARTESIAN_POINT ( 'NONE',  ( -10.88404822699983576, 0.000000000000000000, 29.60989680561421622 ) ) ;
#12512 = CARTESIAN_POINT ( 'NONE',  ( -13.27898586450066709, 3.000000000000000000, 5.170206418547661720 ) ) ;
#12513 = ADVANCED_FACE ( 'NONE', ( #8379 ), #8255, .T. ) ;
#12514 = CARTESIAN_POINT ( 'NONE',  ( 11.90209577080759296, 0.000000000000000000, -8.180229652970856691 ) ) ;
#12515 = LINE ( 'NONE', #10563, #1874 ) ;
#12516 = EDGE_LOOP ( 'NONE', ( #2982, #8225, #8224, #3541 ) ) ;
#12517 = CYLINDRICAL_SURFACE ( 'NONE', #11946, 14.25000000000000000 ) ;
#12518 = ORIENTED_EDGE ( 'NONE', *, *, #3887, .F. ) ;
#12519 = ORIENTED_EDGE ( 'NONE', *, *, #4675, .T. ) ;
#12520 = ORIENTED_EDGE ( 'NONE', *, *, #510, .F. ) ;
#12521 = EDGE_CURVE ( 'NONE', #344, #2254, #12483, .T. ) ;
#12522 = EDGE_CURVE ( 'NONE', #1110, #9161, #7364, .T. ) ;
#12523 = ORIENTED_EDGE ( 'NONE', *, *, #9184, .F. ) ;
#12524 = CARTESIAN_POINT ( 'NONE',  ( -12.40347894490204972, 3.000000000000000000, 3.892776652129660064 ) ) ;
#12525 = CARTESIAN_POINT ( 'NONE',  ( -14.16466328168009881, 3.000000000000000000, 1.557181465540760534 ) ) ;
#12526 = DIRECTION ( 'NONE',  ( 0.000000000000000000, 1.000000000000000000, 0.000000000000000000 ) ) ;
#12527 = ADVANCED_FACE ( 'NONE', ( #5161 ), #9365, .T. ) ;
#12528 = CARTESIAN_POINT ( 'NONE',  ( 6.554160776451332104, 1.734723475976807094E-15, -1.614148852004323231 ) ) ;
#12529 = CARTESIAN_POINT ( 'NONE',  ( 0.000000000000000000, -3.000000000000000000, 0.000000000000000000 ) ) ;
#12530 = ORIENTED_EDGE ( 'NONE', *, *, #8912, .F. ) ;
#12531 = DIRECTION ( 'NONE',  ( 0.000000000000000000, 1.000000000000000000, 0.000000000000000000 ) ) ;
#12532 = FACE_OUTER_BOUND ( 'NONE', #3843, .T. ) ;
#12533 = EDGE_CURVE ( 'NONE', #7268, #2335, #9625, .T. ) ;
#12534 = VERTEX_POINT ( 'NONE', #4328 ) ;
#12535 = CARTESIAN_POINT ( 'NONE',  ( -6.558450276537426404, 0.000000000000000000, -1.596630818375423866 ) ) ;
#12536 = DIRECTION ( 'NONE',  ( -0.000000000000000000, -1.000000000000000000, -0.000000000000000000 ) ) ;
#12537 = CARTESIAN_POINT ( 'NONE',  ( 13.50000000000000355, 3.000000000000000000, -8.549999999999998934 ) ) ;
#12538 = CARTESIAN_POINT ( 'NONE',  ( 10.25006213149504752, 0.000000000000000000, -9.299128225235653744 ) ) ;
#12539 = DIRECTION ( 'NONE',  ( 0.000000000000000000, 1.000000000000000000, -0.000000000000000000 ) ) ;
#12540 = CARTESIAN_POINT ( 'NONE',  ( -12.68816982652953840, 0.000000000000000000, -2.830255545554093644 ) ) ;
#12541 = CARTESIAN_POINT ( 'NONE',  ( -10.34346111134701118, 0.000000000000000000, -8.760376775873707444 ) ) ;
#12542 = ORIENTED_EDGE ( 'NONE', *, *, #866, .T. ) ;
#12543 = EDGE_CURVE ( 'NONE', #11130, #3210, #73, .T. ) ;
#12544 = EDGE_LOOP ( 'NONE', ( #4279, #5485 ) ) ;
#12545 = DIRECTION ( 'NONE',  ( 0.000000000000000000, 0.000000000000000000, 1.000000000000000000 ) ) ;
#12546 = CIRCLE ( 'NONE', #2183, 14.25000000000000178 ) ;
#12547 = EDGE_LOOP ( 'NONE', ( #6781, #12064 ) ) ;
#12548 = CARTESIAN_POINT ( 'NONE',  ( -12.68816982652953840, 3.000000000000000000, -2.830255545554093644 ) ) ;
#12549 = CARTESIAN_POINT ( 'NONE',  ( 30.73000000000000043, 3.000000000000000000, -3.999999999999999112 ) ) ;
#12550 = SURFACE_SIDE_STYLE ('',( #5030 ) ) ;
#12551 = CARTESIAN_POINT ( 'NONE',  ( 0.000000000000000000, 2.900000000000000355, 0.000000000000000000 ) ) ;
#12552 = VECTOR ( 'NONE', #12181, 1000.000000000000000 ) ;
#12553 = CARTESIAN_POINT ( 'NONE',  ( 9.299128225235451239, 3.000000000000000000, -10.25006213149493561 ) ) ;
#12554 = CIRCLE ( 'NONE', #3076, 12.08999999999737440 ) ;
#12555 = CARTESIAN_POINT ( 'NONE',  ( 8.481367827640703183, 9.000000000000000000, 0.5624942419805127880 ) ) ;
#12556 = ORIENTED_EDGE ( 'NONE', *, *, #12477, .F. ) ;
#12557 = FACE_OUTER_BOUND ( 'NONE', #6385, .T. ) ;
#12558 = ORIENTED_EDGE ( 'NONE', *, *, #11390, .F. ) ;
#12559 = EDGE_CURVE ( 'NONE', #11264, #8366, #8051, .T. ) ;
#12560 = ORIENTED_EDGE ( 'NONE', *, *, #7182, .F. ) ;
#12561 = CARTESIAN_POINT ( 'NONE',  ( -4.227250083625790467, 0.000000000000000000, -13.17831234185026013 ) ) ;
#12562 = ORIENTED_EDGE ( 'NONE', *, *, #10739, .F. ) ;
#12563 = AXIS2_PLACEMENT_3D ( 'NONE', #3737, #6918, #9041 ) ;
#12564 = CARTESIAN_POINT ( 'NONE',  ( -5.250000000000000000, 0.000000000000000000, -29.44078293894052933 ) ) ;
#12565 = LINE ( 'NONE', #1253, #8459 ) ;
#12566 = CARTESIAN_POINT ( 'NONE',  ( -5.797378255456022700, 0.000000000000000000, -12.25282671965375592 ) ) ;
#12567 = DIRECTION ( 'NONE',  ( -0.000000000000000000, -1.000000000000000000, -0.000000000000000000 ) ) ;
#12568 = CARTESIAN_POINT ( 'NONE',  ( -10.97318381393799136, 0.000000000000000000, -6.970598036433411693 ) ) ;
#12569 = DIRECTION ( 'NONE',  ( 1.000000000000000000, 0.000000000000000000, 0.000000000000000000 ) ) ;
#12570 = CARTESIAN_POINT ( 'NONE',  ( 2.525608486058770641, 0.09999999999999982514, 2.423076923076923350 ) ) ;
#12571 = LINE ( 'NONE', #2798, #6485 ) ;
#12572 = VERTEX_POINT ( 'NONE', #10730 ) ;
#12573 = CARTESIAN_POINT ( 'NONE',  ( -11.17001009226120445, 3.000000000000000000, -6.660869730750943241 ) ) ;
#12574 = CIRCLE ( 'NONE', #6617, 6.750000000000000888 ) ;
#12575 = ADVANCED_FACE ( 'NONE', ( #8513 ), #11630, .F. ) ;
#12576 = AXIS2_PLACEMENT_3D ( 'NONE', #8375, #12795, #5352 ) ;
#12577 = EDGE_LOOP ( 'NONE', ( #5935, #7383, #5748, #8489 ) ) ;
#12578 = ORIENTED_EDGE ( 'NONE', *, *, #4287, .F. ) ;
#12579 = ORIENTED_EDGE ( 'NONE', *, *, #11874, .F. ) ;
#12580 = EDGE_CURVE ( 'NONE', #8365, #8454, #9138, .T. ) ;
#12581 = EDGE_CURVE ( 'NONE', #5856, #4931, #3856, .T. ) ;
#12582 = ORIENTED_EDGE ( 'NONE', *, *, #8846, .F. ) ;
#12583 = CARTESIAN_POINT ( 'NONE',  ( 7.500000000000003553, 3.000000000000000000, 1.399999999999998579 ) ) ;
#12584 = FILL_AREA_STYLE_COLOUR ( '', #10450 ) ;
#12585 = CIRCLE ( 'NONE', #8588, 3.100000000000000533 ) ;
#12586 = CARTESIAN_POINT ( 'NONE',  ( 0.000000000000000000, 0.000000000000000000, 0.000000000000000000 ) ) ;
#12587 = CARTESIAN_POINT ( 'NONE',  ( 31.00000000000000000, 0.09999999999999982514, -1.500000000000003997 ) ) ;
#12588 = DIRECTION ( 'NONE',  ( -0.9254744032703046130, 0.000000000000000000, -0.3788101488760216018 ) ) ;
#12589 = EDGE_CURVE ( 'NONE', #1159, #6548, #8248, .T. ) ;
#12590 = VERTEX_POINT ( 'NONE', #3418 ) ;
#12591 = ORIENTED_EDGE ( 'NONE', *, *, #8848, .T. ) ;
#12592 = ORIENTED_EDGE ( 'NONE', *, *, #3005, .T. ) ;
#12593 = VECTOR ( 'NONE', #11585, 1000.000000000000000 ) ;
#12594 = DIRECTION ( 'NONE',  ( 0.000000000000000000, 0.000000000000000000, -1.000000000000000000 ) ) ;
#12595 = CARTESIAN_POINT ( 'NONE',  ( 22.00000000000000000, 0.000000000000000000, 0.000000000000000000 ) ) ;
#12596 = ORIENTED_EDGE ( 'NONE', *, *, #4654, .F. ) ;
#12597 = CARTESIAN_POINT ( 'NONE',  ( 0.000000000000000000, 3.000000000000000000, 5.000000000000000000 ) ) ;
#12598 = CLOSED_SHELL ( 'NONE', ( #4109, #3936, #367, #5676, #11245, #12312, #7831, #12244, #8601, #6926, #5236, #2869, #9085, #3212, #8738, #1298, #1583, #433, #12132, #5470, #5756, #4896, #4479, #8519, #12841, #12366, #10767, #10220, #9204, #11593, #9866, #7430, #3484, #2566, #4982, #9890, #11386, #59, #1911, #7679, #878, #3455, #5589, #4389, #7465, #9708, #5742, #10956, #9025, #12797, #3959, #7607, #5981, #10960, #8778, #10867, #1891, #7374, #12977, #7436, #2453, #7029, #153, #13237, #10321, #11834, #1365, #7873, #5936, #7846, #3697, #11811, #11617, #5392, #7935, #13065, #1518, #12724, #13437, #13011, #7454, #917, #6377, #1603, #4114, #8582, #13365, #12236, #10644, #6737, #4397, #957, #11978, #3379, #3279, #3359, #7941 ) ) ;
#12599 = CIRCLE ( 'NONE', #11501, 12.08999999999737440 ) ;
#12600 = CIRCLE ( 'NONE', #69, 12.08999999999737263 ) ;
#12601 = CARTESIAN_POINT ( 'NONE',  ( 0.000000000000000000, 0.000000000000000000, 0.000000000000000000 ) ) ;
#12602 = CARTESIAN_POINT ( 'NONE',  ( 5.733772933379453818, 0.000000000000000000, 13.04554897075800568 ) ) ;
#12603 = DIRECTION ( 'NONE',  ( 0.000000000000000000, 0.000000000000000000, 1.000000000000000000 ) ) ;
#12604 = CARTESIAN_POINT ( 'NONE',  ( -12.68816982652953840, 0.000000000000000000, -2.830255545554093644 ) ) ;
#12605 = EDGE_CURVE ( 'NONE', #2976, #2335, #7630, .T. ) ;
#12606 = CARTESIAN_POINT ( 'NONE',  ( -2.928250210355484828, 0.000000000000000000, -13.52637830886140335 ) ) ;
#12607 = ORIENTED_EDGE ( 'NONE', *, *, #5411, .T. ) ;
#12608 = VECTOR ( 'NONE', #4613, 1000.000000000000000 ) ;
#12609 = ORIENTED_EDGE ( 'NONE', *, *, #10779, .T. ) ;
#12610 = CARTESIAN_POINT ( 'NONE',  ( 0.000000000000000000, 3.000000000000000000, 0.000000000000000000 ) ) ;
#12611 = AXIS2_PLACEMENT_3D ( 'NONE', #12549, #7110, #11310 ) ;
#12612 = CIRCLE ( 'NONE', #6656, 1.600000000000004086 ) ;
#12613 = VERTEX_POINT ( 'NONE', #7427 ) ;
#12614 = CARTESIAN_POINT ( 'NONE',  ( -6.515098946627274401, 0.000000000000000000, 3.430563300314522390 ) ) ;
#12615 = CARTESIAN_POINT ( 'NONE',  ( -11.52662650599083882, 0.000000000000000000, 3.647599401157695986 ) ) ;
#12616 = CARTESIAN_POINT ( 'NONE',  ( 3.893011711613070691, 0.000000000000000000, -12.40340517008307231 ) ) ;
#12617 = AXIS2_PLACEMENT_3D ( 'NONE', #12595, #12474, #7220 ) ;
#12618 = CARTESIAN_POINT ( 'NONE',  ( -9.379342464487789854, 0.000000000000000000, -10.98198414889931307 ) ) ;
#12619 = PRODUCT ( 'base-mounting-bracket', 'base-mounting-bracket', '', ( #12479 ) ) ;
#12620 = AXIS2_PLACEMENT_3D ( 'NONE', #478, #3775, #10051 ) ;
#12621 = CARTESIAN_POINT ( 'NONE',  ( -2.976187484161006314, 0.000000000000000000, 7.363908159724035229 ) ) ;
#12622 = CARTESIAN_POINT ( 'NONE',  ( 46.02418392430381999, 3.000000000000000000, -15.41988256844266836 ) ) ;
#12623 = CIRCLE ( 'NONE', #2494, 9.250000000000000000 ) ;
#12624 = EDGE_LOOP ( 'NONE', ( #12950, #6792, #12908, #2461 ) ) ;
#12625 = CARTESIAN_POINT ( 'NONE',  ( -2.655466033450426533, 9.000000000000000000, -7.485541762018160128 ) ) ;
#12626 = VERTEX_POINT ( 'NONE', #11693 ) ;
#12627 = ORIENTED_EDGE ( 'NONE', *, *, #9366, .F. ) ;
#12628 = VERTEX_POINT ( 'NONE', #11833 ) ;
#12629 = CARTESIAN_POINT ( 'NONE',  ( 0.000000000000000000, 0.000000000000000000, 0.000000000000000000 ) ) ;
#12630 = ORIENTED_EDGE ( 'NONE', *, *, #11635, .F. ) ;
#12631 = AXIS2_PLACEMENT_3D ( 'NONE', #10511, #11550, #9467 ) ;
#12632 = CARTESIAN_POINT ( 'NONE',  ( -11.80615107470192804, 0.000000000000000000, -2.604399508764160487 ) ) ;
#12633 = CARTESIAN_POINT ( 'NONE',  ( 9.325031192972383920, 3.000000000000000000, -9.065266643391169055 ) ) ;
#12634 = LINE ( 'NONE', #13592, #11716 ) ;
#12635 = CARTESIAN_POINT ( 'NONE',  ( 54.70014691233865989, 3.000000000000000000, -3.785783530882224746 ) ) ;
#12636 = EDGE_CURVE ( 'NONE', #2659, #11402, #12976, .T. ) ;
#12637 = CARTESIAN_POINT ( 'NONE',  ( 8.252687871541629860, 3.000000000000000000, 31.00000000000000000 ) ) ;
#12638 = CARTESIAN_POINT ( 'NONE',  ( -5.571313494980134173, 0.000000000000000000, 10.72979803820131295 ) ) ;
#12639 = DIRECTION ( 'NONE',  ( -3.491481338843133355E-15, -1.000000000000000000, 9.085131966639173460E-31 ) ) ;
#12640 = CARTESIAN_POINT ( 'NONE',  ( -2.161962830978702677, 3.000000000000000000, 14.08504230442587435 ) ) ;
#12641 = ORIENTED_EDGE ( 'NONE', *, *, #4536, .T. ) ;
#12642 = AXIS2_PLACEMENT_3D ( 'NONE', #10994, #1496, #12184 ) ;
#12643 = CARTESIAN_POINT ( 'NONE',  ( 11.46814821560793618, 0.000000000000000000, -5.731782959214992701 ) ) ;
#12644 = AXIS2_PLACEMENT_3D ( 'NONE', #4271, #4472, #8466 ) ;
#12645 = VERTEX_POINT ( 'NONE', #4528 ) ;
#12646 = ORIENTED_EDGE ( 'NONE', *, *, #10197, .T. ) ;
#12647 = ORIENTED_EDGE ( 'NONE', *, *, #6320, .F. ) ;
#12648 = EDGE_LOOP ( 'NONE', ( #12560, #2443, #10504, #7887, #10122, #3972, #6226, #10709 ) ) ;
#12649 = CARTESIAN_POINT ( 'NONE',  ( -7.235926821844430812, 9.000000000000000000, 4.459973433655439301 ) ) ;
#12650 = VECTOR ( 'NONE', #6317, 1000.000000000000000 ) ;
#12651 = LINE ( 'NONE', #10573, #11544 ) ;
#12652 = EDGE_CURVE ( 'NONE', #1554, #10329, #12800, .T. ) ;
#12653 = DIRECTION ( 'NONE',  ( 0.000000000000000000, 0.000000000000000000, 1.000000000000000000 ) ) ;
#12654 = CARTESIAN_POINT ( 'NONE',  ( -11.48836750521723893, 3.000000000000000000, 8.430890348300625448 ) ) ;
#12655 = DIRECTION ( 'NONE',  ( -0.000000000000000000, -1.000000000000000000, -0.000000000000000000 ) ) ;
#12656 = EDGE_CURVE ( 'NONE', #12211, #8258, #7386, .T. ) ;
#12657 = CARTESIAN_POINT ( 'NONE',  ( 9.250000000000003553, 2.750000000000000888, 10.00000000000000000 ) ) ;
#12658 = ADVANCED_FACE ( 'NONE', ( #6382 ), #6716, .T. ) ;
#12659 = ORIENTED_EDGE ( 'NONE', *, *, #4582, .T. ) ;
#12660 =( GEOMETRIC_REPRESENTATION_CONTEXT ( 3 ) GLOBAL_UNCERTAINTY_ASSIGNED_CONTEXT ( ( #9291 ) ) GLOBAL_UNIT_ASSIGNED_CONTEXT ( ( #11929, #5926, #12353 ) ) REPRESENTATION_CONTEXT ( 'NONE', 'WORKASPACE' ) );
#12661 = VECTOR ( 'NONE', #5034, 1000.000000000000000 ) ;
#12662 = ORIENTED_EDGE ( 'NONE', *, *, #13491, .F. ) ;
#12663 = LINE ( 'NONE', #1146, #4657 ) ;
#12664 = EDGE_LOOP ( 'NONE', ( #10484, #9696, #5091, #145 ) ) ;
#12665 = DIRECTION ( 'NONE',  ( -0.000000000000000000, -1.000000000000000000, -0.000000000000000000 ) ) ;
#12666 = EDGE_CURVE ( 'NONE', #11420, #4097, #10247, .T. ) ;
#12667 = DIRECTION ( 'NONE',  ( -0.000000000000000000, -1.000000000000000000, 0.000000000000000000 ) ) ;
#12668 = MECHANICAL_DESIGN_GEOMETRIC_PRESENTATION_REPRESENTATION (  '', ( #2987 ), #11350 ) ;
#12669 = AXIS2_PLACEMENT_3D ( 'NONE', #202, #10671, #5421 ) ;
#12670 = LINE ( 'NONE', #7291, #13003 ) ;
#12671 = CARTESIAN_POINT ( 'NONE',  ( 13.27898586450069907, 0.000000000000000000, 5.170206418547587113 ) ) ;
#12672 = LINE ( 'NONE', #72, #9555 ) ;
#12673 = EDGE_CURVE ( 'NONE', #7170, #13219, #12208, .T. ) ;
#12674 = CARTESIAN_POINT ( 'NONE',  ( -8.890701948131944476, 3.000000000000000000, 13.39999999999999858 ) ) ;
#12675 = B_SPLINE_CURVE_WITH_KNOTS ( 'NONE', 3,
 ( #12321, #813, #2862, #7074 ),
 .UNSPECIFIED., .F., .F.,
 ( 4, 4 ),
 ( 0.1276832474596270861, 1.000000000000000000 ),
 .UNSPECIFIED. ) ;
#12676 = SURFACE_SIDE_STYLE ('',( #10731 ) ) ;
#12677 = B_SPLINE_CURVE_WITH_KNOTS ( 'NONE', 3,
 ( #908, #9504, #5179, #13518 ),
 .UNSPECIFIED., .F., .F.,
 ( 4, 4 ),
 ( 0.000000000000000000, 0.5855695330273008592 ),
 .UNSPECIFIED. ) ;
#12678 = ORIENTED_EDGE ( 'NONE', *, *, #6864, .T. ) ;
#12679 = VERTEX_POINT ( 'NONE', #6527 ) ;
#12680 = PRODUCT_DEFINITION_FORMATION_WITH_SPECIFIED_SOURCE ( 'ANY', '', #12619, .NOT_KNOWN. ) ;
#12681 = VERTEX_POINT ( 'NONE', #1289 ) ;
#12682 = DIRECTION ( 'NONE',  ( -0.000000000000000000, -1.000000000000000000, -0.000000000000000000 ) ) ;
#12683 = VERTEX_POINT ( 'NONE', #9686 ) ;
#12684 = ADVANCED_FACE ( 'NONE', ( #263 ), #4454, .F. ) ;
#12685 = FACE_BOUND ( 'NONE', #9813, .T. ) ;
#12686 =( NAMED_UNIT ( * ) PLANE_ANGLE_UNIT ( ) SI_UNIT ( $, .RADIAN. ) );
#12687 = CARTESIAN_POINT ( 'NONE',  ( -12.14623037080100865, 3.000000000000000000, 4.072642252455982437 ) ) ;
#12688 = CARTESIAN_POINT ( 'NONE',  ( 3.000000000000001776, 2.000000000000000000, 10.00000000000000000 ) ) ;
#12689 = CYLINDRICAL_SURFACE ( 'NONE', #7776, 12.08999999999737440 ) ;
#12690 = CARTESIAN_POINT ( 'NONE',  ( -9.133371500908470608, 3.000000000000000000, -11.90284147956855065 ) ) ;
#12691 =( REPRESENTATION_RELATIONSHIP ('NONE','NONE', #3798, #8461 ) REPRESENTATION_RELATIONSHIP_WITH_TRANSFORMATION ( #995 )SHAPE_REPRESENTATION_RELATIONSHIP( ) );
#12692 = LINE ( 'NONE', #156, #1355 ) ;
#12693 = CARTESIAN_POINT ( 'NONE',  ( -3.647599401157625376, 0.000000000000000000, -11.52662650599085836 ) ) ;
#12694 = ORIENTED_EDGE ( 'NONE', *, *, #885, .T. ) ;
#12695 = VERTEX_POINT ( 'NONE', #8849 ) ;
#12696 = ORIENTED_EDGE ( 'NONE', *, *, #2733, .F. ) ;
#12697 = VERTEX_POINT ( 'NONE', #12108 ) ;
#12698 = DIRECTION ( 'NONE',  ( 0.000000000000000000, 0.000000000000000000, 1.000000000000000000 ) ) ;
#12699 = ORIENTED_EDGE ( 'NONE', *, *, #11806, .F. ) ;
#12700 = CARTESIAN_POINT ( 'NONE',  ( 0.5501230721522984979, 3.000000000000000000, -12.98835496148321766 ) ) ;
#12701 = CARTESIAN_POINT ( 'NONE',  ( 12.63269908545826503, 3.000000000000000000, -5.340493616518841691 ) ) ;
#12702 = CARTESIAN_POINT ( 'NONE',  ( 0.000000000000000000, 3.000000000000000000, 0.000000000000000000 ) ) ;
#12703 = FACE_OUTER_BOUND ( 'NONE', #11770, .T. ) ;
#12704 = DIRECTION ( 'NONE',  ( -0.000000000000000000, -1.000000000000000000, -0.000000000000000000 ) ) ;
#12705 = CARTESIAN_POINT ( 'NONE',  ( 13.50000000000000355, 3.000000000000000000, -7.050000000000000711 ) ) ;
#12706 = PLANE ( 'NONE',  #9564 ) ;
#12707 = VERTEX_POINT ( 'NONE', #9823 ) ;
#12708 = DIRECTION ( 'NONE',  ( 0.000000000000000000, 0.000000000000000000, 1.000000000000000000 ) ) ;
#12709 = PRODUCT_DEFINITION_SHAPE ( 'NONE', 'NONE',  #10179 ) ;
#12710 = ORIENTED_EDGE ( 'NONE', *, *, #2119, .F. ) ;
#12711 = ORIENTED_EDGE ( 'NONE', *, *, #5648, .F. ) ;
#12712 = EDGE_CURVE ( 'NONE', #2029, #10212, #6728, .T. ) ;
#12713 = ORIENTED_EDGE ( 'NONE', *, *, #3956, .T. ) ;
#12714 = CARTESIAN_POINT ( 'NONE',  ( -14.39763212228012534, 0.000000000000000000, 1.133238802859812155 ) ) ;
#12715 = CYLINDRICAL_SURFACE ( 'NONE', #1391, 3.000000000000000888 ) ;
#12716 = CARTESIAN_POINT ( 'NONE',  ( 12.08646469655232636, 3.000000000000000000, -8.883544964652022813 ) ) ;
#12717 = LINE ( 'NONE', #2314, #6187 ) ;
#12718 = CARTESIAN_POINT ( 'NONE',  ( -4.056222772158361245, 3.000000000000000000, 12.16218796965919324 ) ) ;
#12719 = VERTEX_POINT ( 'NONE', #604 ) ;
#12720 = ORIENTED_EDGE ( 'NONE', *, *, #13266, .T. ) ;
#12721 = EDGE_CURVE ( 'NONE', #1968, #1592, #5583, .T. ) ;
#12722 = CARTESIAN_POINT ( 'NONE',  ( 4.201465772524378472, 9.000000000000000000, 6.047394330962382547 ) ) ;
#12723 = EDGE_CURVE ( 'NONE', #1584, #6498, #8014, .T. ) ;
#12724 = ADVANCED_FACE ( 'NONE', ( #13200 ), #2657, .T. ) ;
#12725 = EDGE_LOOP ( 'NONE', ( #2614, #5632, #7079, #9218 ) ) ;
#12726 = CARTESIAN_POINT ( 'NONE',  ( -12.40347894490204794, 0.000000000000000000, 3.892776652129663173 ) ) ;
#12727 = EDGE_CURVE ( 'NONE', #10584, #20, #759, .T. ) ;
#12728 = DIRECTION ( 'NONE',  ( 0.000000000000000000, 1.000000000000000000, 0.000000000000000000 ) ) ;
#12729 = FACE_OUTER_BOUND ( 'NONE', #13385, .T. ) ;
#12730 = FACE_OUTER_BOUND ( 'NONE', #7840, .T. ) ;
#12731 = CARTESIAN_POINT ( 'NONE',  ( -11.52662650599092409, 3.000000000000000000, 3.647599401157420651 ) ) ;
#12732 = DIRECTION ( 'NONE',  ( 0.000000000000000000, 1.000000000000000000, 0.000000000000000000 ) ) ;
#12733 = B_SPLINE_CURVE_WITH_KNOTS ( 'NONE', 3,
 ( #6755, #9094, #13103, #6894 ),
 .UNSPECIFIED., .F., .F.,
 ( 4, 4 ),
 ( 0.1276832474596353850, 1.000000000000000000 ),
 .UNSPECIFIED. ) ;
#12734 = CARTESIAN_POINT ( 'NONE',  ( 4.821006024660968947, 0.000000000000000000, -13.61374091949021015 ) ) ;
#12735 = EDGE_CURVE ( 'NONE', #12863, #12205, #10095, .T. ) ;
#12736 = ORIENTED_EDGE ( 'NONE', *, *, #5607, .T. ) ;
#12737 = EDGE_LOOP ( 'NONE', ( #2684, #13470, #12151, #12435 ) ) ;
#12738 = ORIENTED_EDGE ( 'NONE', *, *, #857, .T. ) ;
#12739 = DIRECTION ( 'NONE',  ( 0.000000000000000000, 1.000000000000000000, -0.000000000000000000 ) ) ;
#12740 = ORIENTED_EDGE ( 'NONE', *, *, #3807, .F. ) ;
#12741 = EDGE_CURVE ( 'NONE', #1513, #5397, #8037, .T. ) ;
#12742 = EDGE_CURVE ( 'NONE', #8751, #6867, #3835, .T. ) ;
#12743 = FACE_BOUND ( 'NONE', #6885, .T. ) ;
#12744 = DIRECTION ( 'NONE',  ( -0.000000000000000000, -1.000000000000000000, -0.000000000000000000 ) ) ;
#12745 = CARTESIAN_POINT ( 'NONE',  ( -7.780961115628980629, 9.000000000000000000, -3.421497350147988392 ) ) ;
#12746 = CARTESIAN_POINT ( 'NONE',  ( -6.558450276537426404, 0.000000000000000000, -1.596630818375420757 ) ) ;
#12747 = DIRECTION ( 'NONE',  ( 0.000000000000000000, 0.000000000000000000, -1.000000000000000000 ) ) ;
#12748 = CARTESIAN_POINT ( 'NONE',  ( 11.63517940784358196, 0.000000000000000000, -7.494008246337187096 ) ) ;
#12749 = VERTEX_POINT ( 'NONE', #11068 ) ;
#12750 =( LENGTH_UNIT ( ) NAMED_UNIT ( * ) SI_UNIT ( .MILLI., .METRE. ) );
#12751 = EDGE_LOOP ( 'NONE', ( #3012, #10085, #1144, #10687 ) ) ;
#12752 = ORIENTED_EDGE ( 'NONE', *, *, #1620, .F. ) ;
#12753 = AXIS2_PLACEMENT_3D ( 'NONE', #6266, #10477, #1035 ) ;
#12754 = ADVANCED_FACE ( 'NONE', ( #396, #6788 ), #10929, .F. ) ;
#12755 = ORIENTED_EDGE ( 'NONE', *, *, #2752, .T. ) ;
#12756 = CARTESIAN_POINT ( 'NONE',  ( -6.549210654805285081, 0.000000000000000000, 1.634117437329677180 ) ) ;
#12757 = VERTEX_POINT ( 'NONE', #2593 ) ;
#12758 = LINE ( 'NONE', #1117, #11768 ) ;
#12759 = DIRECTION ( 'NONE',  ( -0.000000000000000000, -1.000000000000000000, -0.000000000000000000 ) ) ;
#12760 = TOROIDAL_SURFACE ( 'NONE', #7905, 3.399999999999999911, 0.1000000000000000056 ) ;
#12761 = FACE_OUTER_BOUND ( 'NONE', #13341, .T. ) ;
#12762 = DIRECTION ( 'NONE',  ( 0.000000000000000000, 0.000000000000000000, -1.000000000000000000 ) ) ;
#12763 = AXIS2_PLACEMENT_3D ( 'NONE', #7356, #12728, #954 ) ;
#12764 = DIRECTION ( 'NONE',  ( 0.000000000000000000, -0.000000000000000000, 1.000000000000000000 ) ) ;
#12765 = CARTESIAN_POINT ( 'NONE',  ( -13.52637830886139092, 0.000000000000000000, 2.928250210355532790 ) ) ;
#12766 = CARTESIAN_POINT ( 'NONE',  ( 9.593885948927676210, 3.000000000000000000, -8.504652361247169168 ) ) ;
#12767 = CARTESIAN_POINT ( 'NONE',  ( 11.48836750521724070, 3.000000000000000000, -8.430890348300621895 ) ) ;
#12768 = ORIENTED_EDGE ( 'NONE', *, *, #4056, .F. ) ;
#12769 = CARTESIAN_POINT ( 'NONE',  ( -8.369528376005813897, 0.000000000000000000, 1.483574994138652903 ) ) ;
#12770 = EDGE_CURVE ( 'NONE', #1091, #11589, #5365, .T. ) ;
#12771 = VERTEX_POINT ( 'NONE', #9885 ) ;
#12772 = ADVANCED_FACE ( 'NONE', ( #12258 ), #7008, .F. ) ;
#12773 = ORIENTED_EDGE ( 'NONE', *, *, #10209, .T. ) ;
#12774 = VECTOR ( 'NONE', #10081, 1000.000000000000000 ) ;
#12775 = VECTOR ( 'NONE', #7834, 1000.000000000000000 ) ;
#12776 = EDGE_LOOP ( 'NONE', ( #4276, #9661, #13371, #10969 ) ) ;
#12777 = CARTESIAN_POINT ( 'NONE',  ( -0.4399887592034530392, 9.000000000000000000, 8.488604708182295511 ) ) ;
#12778 = CARTESIAN_POINT ( 'NONE',  ( -0.5398653231797316820, 0.000000000000000000, 12.07794044664754018 ) ) ;
#12779 = CARTESIAN_POINT ( 'NONE',  ( -6.549210654805285969, 0.000000000000000000, 1.634117437329680067 ) ) ;
#12780 = CIRCLE ( 'NONE', #5960, 6.749999999999999112 ) ;
#12781 = DIRECTION ( 'NONE',  ( -0.000000000000000000, -1.000000000000000000, -0.000000000000000000 ) ) ;
#12782 = CARTESIAN_POINT ( 'NONE',  ( 31.00000000000000000, 0.000000000000000000, 3.999999998926329514 ) ) ;
#12783 = VECTOR ( 'NONE', #13147, 1000.000000000000000 ) ;
#12784 = DIRECTION ( 'NONE',  ( 0.000000000000000000, 0.000000000000000000, -1.000000000000000000 ) ) ;
#12785 = VERTEX_POINT ( 'NONE', #11202 ) ;
#12786 = VERTEX_POINT ( 'NONE', #11141 ) ;
#12787 = ADVANCED_BREP_SHAPE_REPRESENTATION ( '', ( #8836, #10007 ), #5191 ) ;
#12788 = CARTESIAN_POINT ( 'NONE',  ( -20.56403552112892896, 3.000000000000000000, -16.70078978407140013 ) ) ;
#12789 = B_SPLINE_CURVE_WITH_KNOTS ( 'NONE', 2,
 ( #6491, #4210, #10559 ),
 .UNSPECIFIED., .F., .F.,
 ( 3, 3 ),
 ( 0.000000000000000000, 1.000000000000000000 ),
 .UNSPECIFIED. ) ;
#12790 = AXIS2_PLACEMENT_3D ( 'NONE', #7475, #7544, #8628 ) ;
#12791 = VECTOR ( 'NONE', #1352, 1000.000000000000000 ) ;
#12792 = ORIENTED_EDGE ( 'NONE', *, *, #12949, .F. ) ;
#12793 = CARTESIAN_POINT ( 'NONE',  ( -10.33484986938308303, 0.000000000000000000, 8.771102293099071190 ) ) ;
#12794 = CYLINDRICAL_SURFACE ( 'NONE', #8786, 12.08999999999737440 ) ;
#12795 = DIRECTION ( 'NONE',  ( -0.000000000000000000, -1.000000000000000000, -0.000000000000000000 ) ) ;
#12796 = CARTESIAN_POINT ( 'NONE',  ( -12.16218796965919324, 0.000000000000000000, -4.056222772158363021 ) ) ;
#12797 = ADVANCED_FACE ( 'NONE', ( #459 ), #4660, .T. ) ;
#12798 = CARTESIAN_POINT ( 'NONE',  ( 11.99999999999999289, -4.861632610112956756E-14, -3.122502256758250798E-15 ) ) ;
#12799 = AXIS2_PLACEMENT_3D ( 'NONE', #6222, #859, #1058 ) ;
#12800 = LINE ( 'NONE', #3221, #4964 ) ;
#12801 = DIRECTION ( 'NONE',  ( -1.000000000000000000, 0.000000000000000000, -0.000000000000000000 ) ) ;
#12802 = VERTEX_POINT ( 'NONE', #3624 ) ;
#12803 = ORIENTED_EDGE ( 'NONE', *, *, #11345, .F. ) ;
#12804 = ORIENTED_EDGE ( 'NONE', *, *, #9113, .T. ) ;
#12805 = CARTESIAN_POINT ( 'NONE',  ( 0.000000000000000000, 3.000000000000000000, 0.000000000000000000 ) ) ;
#12806 = ORIENTED_EDGE ( 'NONE', *, *, #1541, .T. ) ;
#12807 = AXIS2_PLACEMENT_3D ( 'NONE', #11416, #5213, #12594 ) ;
#12808 = DIRECTION ( 'NONE',  ( -0.000000000000000000, -1.000000000000000000, -0.000000000000000000 ) ) ;
#12809 = B_SPLINE_SURFACE_WITH_KNOTS ( 'NONE', 3, 1, ( 
 ( #5322, #7139 ),
 ( #8221, #4296 ),
 ( #11605, #12643 ),
 ( #1905, #6098 ) ),
 .UNSPECIFIED., .F., .F., .F.,
 ( 4, 4 ),
 ( 2, 2 ),
 ( 0.000000000000000000, 0.8452273900860258760 ),
 ( 0.000000000000000000, 1.000000000000000000 ),
 .UNSPECIFIED. ) ;
#12810 = EDGE_CURVE ( 'NONE', #1004, #7453, #7824, .T. ) ;
#12811 = CARTESIAN_POINT ( 'NONE',  ( -11.80612203322752585, 0.000000000000000000, 2.604531154829235362 ) ) ;
#12812 = CARTESIAN_POINT ( 'NONE',  ( -9.375397774054503586, 3.000000000000000000, -11.70905276178452503 ) ) ;
#12813 = CARTESIAN_POINT ( 'NONE',  ( 2.620242232815953809, 0.000000000000000000, 6.881105251569436199 ) ) ;
#12814 = DIRECTION ( 'NONE',  ( -0.000000000000000000, -1.000000000000000000, -0.000000000000000000 ) ) ;
#12815 = DIRECTION ( 'NONE',  ( 0.000000000000000000, 1.000000000000000000, 0.000000000000000000 ) ) ;
#12816 = EDGE_LOOP ( 'NONE', ( #2408, #9816, #11961, #8275 ) ) ;
#12817 = VECTOR ( 'NONE', #12987, 1000.000000000000000 ) ;
#12818 = EDGE_CURVE ( 'NONE', #5500, #2426, #10834, .T. ) ;
#12819 = LINE ( 'NONE', #10808, #10631 ) ;
#12820 = ORIENTED_EDGE ( 'NONE', *, *, #321, .F. ) ;
#12821 = AXIS2_PLACEMENT_3D ( 'NONE', #10495, #3185, #7394 ) ;
#12822 = EDGE_CURVE ( 'NONE', #12313, #1251, #4862, .T. ) ;
#12823 = VECTOR ( 'NONE', #9599, 1000.000000000000000 ) ;
#12824 = ORIENTED_EDGE ( 'NONE', *, *, #24, .F. ) ;
#12825 = ORIENTED_EDGE ( 'NONE', *, *, #10574, .T. ) ;
#12826 = CARTESIAN_POINT ( 'NONE',  ( 0.000000000000000000, -3.000000000000000000, 9.250000000000000000 ) ) ;
#12827 = ORIENTED_EDGE ( 'NONE', *, *, #6084, .T. ) ;
#12828 = LINE ( 'NONE', #3380, #7365 ) ;
#12829 = CIRCLE ( 'NONE', #10187, 1.600000000000004086 ) ;
#12830 = SURFACE_SIDE_STYLE ('',( #6622 ) ) ;
#12831 = VECTOR ( 'NONE', #5036, 1000.000000000000000 ) ;
#12832 = CARTESIAN_POINT ( 'NONE',  ( 2.830255545554135832, 3.000000000000000000, -12.68816982652952596 ) ) ;
#12833 = EDGE_CURVE ( 'NONE', #1887, #10439, #4939, .T. ) ;
#12834 = DIRECTION ( 'NONE',  ( 0.000000000000000000, 1.000000000000000000, 2.891205793294684736E-16 ) ) ;
#12835 = DIRECTION ( 'NONE',  ( 0.000000000000000000, 1.000000000000000000, 0.000000000000000000 ) ) ;
#12836 = CARTESIAN_POINT ( 'NONE',  ( 2.631756770590782057, 3.000000000000000000, -14.20034848914875347 ) ) ;
#12837 = CARTESIAN_POINT ( 'NONE',  ( -0.4399887592034473771, 9.000000000000000000, 8.488604708182295511 ) ) ;
#12838 = DIRECTION ( 'NONE',  ( 0.6291930273683233876, 0.000000000000000000, -0.7772490812545771455 ) ) ;
#12839 = ORIENTED_EDGE ( 'NONE', *, *, #7746, .F. ) ;
#12840 = CARTESIAN_POINT ( 'NONE',  ( 6.660877044263387781, 3.000000000000000000, -11.16999893002129696 ) ) ;
#12841 = ADVANCED_FACE ( 'NONE', ( #11413 ), #11705, .F. ) ;
#12842 = ORIENTED_EDGE ( 'NONE', *, *, #5758, .F. ) ;
#12843 = VECTOR ( 'NONE', #734, 1000.000000000000000 ) ;
#12844 = ORIENTED_EDGE ( 'NONE', *, *, #7272, .T. ) ;
#12845 = VECTOR ( 'NONE', #11046, 1000.000000000000000 ) ;
#12846 = CIRCLE ( 'NONE', #312, 0.09999999999999982514 ) ;
#12847 = AXIS2_PLACEMENT_3D ( 'NONE', #645, #13113, #3524 ) ;
#12848 = ORIENTED_EDGE ( 'NONE', *, *, #12349, .F. ) ;
#12849 = DIRECTION ( 'NONE',  ( 0.000000000000000000, 1.000000000000000000, -0.000000000000000000 ) ) ;
#12850 = DIRECTION ( 'NONE',  ( 0.000000000000000000, 0.000000000000000000, 1.000000000000000000 ) ) ;
#12851 = EDGE_CURVE ( 'NONE', #12757, #12500, #326, .T. ) ;
#12852 = EDGE_CURVE ( 'NONE', #13387, #12719, #9196, .T. ) ;
#12853 = DIRECTION ( 'NONE',  ( 1.000000000000000000, 0.000000000000000000, 0.000000000000000000 ) ) ;
#12854 = DIRECTION ( 'NONE',  ( -0.7772490812546168915, 0.000000000000000000, -0.6291930273682743158 ) ) ;
#12855 = CARTESIAN_POINT ( 'NONE',  ( -2.264806262022998062, 3.000000000000000000, -14.82803603298499340 ) ) ;
#12856 = FACE_OUTER_BOUND ( 'NONE', #10751, .T. ) ;
#12857 = EDGE_CURVE ( 'NONE', #7299, #8075, #2509, .T. ) ;
#12858 = ORIENTED_EDGE ( 'NONE', *, *, #113, .F. ) ;
#12859 = VERTEX_POINT ( 'NONE', #13482 ) ;
#12860 = CYLINDRICAL_SURFACE ( 'NONE', #3999, 2.999999999999999112 ) ;
#12861 = VECTOR ( 'NONE', #3964, 1000.000000000000000 ) ;
#12862 = CIRCLE ( 'NONE', #2736, 0.1000000000000000472 ) ;
#12863 = VERTEX_POINT ( 'NONE', #11351 ) ;
#12864 = CARTESIAN_POINT ( 'NONE',  ( 8.883544964651964193, 3.000000000000000000, -12.08646469655236544 ) ) ;
#12865 = CARTESIAN_POINT ( 'NONE',  ( -13.73660796332618261, 3.000000000000000000, -6.025412986832017204 ) ) ;
#12866 = B_SPLINE_CURVE_WITH_KNOTS ( 'NONE', 3,
 ( #5050, #1830, #3944, #9247 ),
 .UNSPECIFIED., .F., .F.,
 ( 4, 4 ),
 ( 0.000000000000000000, 0.5855695330273008592 ),
 .UNSPECIFIED. ) ;
#12867 = CARTESIAN_POINT ( 'NONE',  ( 0.000000000000000000, 9.000000000000000000, 0.000000000000000000 ) ) ;
#12868 = CYLINDRICAL_SURFACE ( 'NONE', #3749, 1.500000000000003997 ) ;
#12869=STYLED_ITEM('',(#13656),#13099);
#12870 = DIRECTION ( 'NONE',  ( 0.000000000000000000, 1.000000000000000000, -0.000000000000000000 ) ) ;
#12871 = VECTOR ( 'NONE', #1883, 1000.000000000000000 ) ;
#12872 = CARTESIAN_POINT ( 'NONE',  ( 26.30958424017656938, 0.09999999999999982514, -1.399999999999999467 ) ) ;
#12873 = AXIS2_PLACEMENT_3D ( 'NONE', #1252, #3244, #6554 ) ;
#12874 = CARTESIAN_POINT ( 'NONE',  ( -6.970598036433426792, 0.000000000000000000, -10.97318381393771780 ) ) ;
#12875 = VERTEX_POINT ( 'NONE', #8302 ) ;
#12876 = ORIENTED_EDGE ( 'NONE', *, *, #1015, .F. ) ;
#12877 = B_SPLINE_CURVE_WITH_KNOTS ( 'NONE', 3,
 ( #9828, #8656, #9695, #7496 ),
 .UNSPECIFIED., .F., .F.,
 ( 4, 4 ),
 ( 0.1547128134717859205, 1.000000000000000000 ),
 .UNSPECIFIED. ) ;
#12878 = ORIENTED_EDGE ( 'NONE', *, *, #9888, .F. ) ;
#12879 = ORIENTED_EDGE ( 'NONE', *, *, #11317, .F. ) ;
#12880 = DIRECTION ( 'NONE',  ( 0.000000000000000000, 0.000000000000000000, 1.000000000000000000 ) ) ;
#12881 = ADVANCED_FACE ( 'NONE', ( #8103 ), #2864, .F. ) ;
#12882 = EDGE_LOOP ( 'NONE', ( #10970, #11014, #6900, #7763 ) ) ;
#12883 =( GEOMETRIC_REPRESENTATION_CONTEXT ( 3 ) GLOBAL_UNCERTAINTY_ASSIGNED_CONTEXT ( ( #4059 ) ) GLOBAL_UNIT_ASSIGNED_CONTEXT ( ( #5864, #10062, #13232 ) ) REPRESENTATION_CONTEXT ( 'NONE', 'WORKASPACE' ) );
#12884 = AXIS2_PLACEMENT_3D ( 'NONE', #10049, #4681, #621 ) ;
#12885 = DIRECTION ( 'NONE',  ( 0.000000000000000000, 0.000000000000000000, 1.000000000000000000 ) ) ;
#12886 = DIRECTION ( 'NONE',  ( 0.000000000000000000, -1.000000000000000000, 0.000000000000000000 ) ) ;
#12887 = CARTESIAN_POINT ( 'NONE',  ( -5.999999999999991118, 3.000000000000000000, 27.00000000000000000 ) ) ;
#12888 = CARTESIAN_POINT ( 'NONE',  ( -2.590203375110137873, 0.000000000000000000, 6.893050072893555758 ) ) ;
#12889 = LINE ( 'NONE', #8667, #9360 ) ;
#12890 = ORIENTED_EDGE ( 'NONE', *, *, #3263, .T. ) ;
#12891 = FACE_OUTER_BOUND ( 'NONE', #2947, .T. ) ;
#12892 = ORIENTED_EDGE ( 'NONE', *, *, #9144, .F. ) ;
#12893 = VERTEX_POINT ( 'NONE', #1919 ) ;
#12894 = ORIENTED_EDGE ( 'NONE', *, *, #5264, .F. ) ;
#12895 = DIRECTION ( 'NONE',  ( 0.4933917819034832619, -0.000000000000000000, -0.8698071910200015910 ) ) ;
#12896 = EDGE_CURVE ( 'NONE', #13143, #2239, #5071, .T. ) ;
#12897 = EDGE_CURVE ( 'NONE', #3201, #12045, #9986, .T. ) ;
#12898 = ORIENTED_EDGE ( 'NONE', *, *, #13410, .T. ) ;
#12899 = ORIENTED_EDGE ( 'NONE', *, *, #9388, .T. ) ;
#12900 = CARTESIAN_POINT ( 'NONE',  ( 9.249999999999996447, -1.734723475976807094E-15, -10.00000000000000178 ) ) ;
#12901 = DIRECTION ( 'NONE',  ( -0.000000000000000000, -1.000000000000000000, -0.000000000000000000 ) ) ;
#12902 = EDGE_CURVE ( 'NONE', #12046, #8060, #9583, .T. ) ;
#12903 = DIRECTION ( 'NONE',  ( -0.000000000000000000, -1.000000000000000000, -0.000000000000000000 ) ) ;
#12904 = CARTESIAN_POINT ( 'NONE',  ( 0.000000000000000000, 3.000000000000000000, 0.000000000000000000 ) ) ;
#12905 = LINE ( 'NONE', #2421, #8867 ) ;
#12906 = CARTESIAN_POINT ( 'NONE',  ( -9.593885948927676210, 3.000000000000000000, 8.504652361247165615 ) ) ;
#12907 = DIRECTION ( 'NONE',  ( 0.000000000000000000, 1.000000000000000000, 0.000000000000000000 ) ) ;
#12908 = ORIENTED_EDGE ( 'NONE', *, *, #11508, .F. ) ;
#12909 = CARTESIAN_POINT ( 'NONE',  ( 6.017756925049591921, 0.000000000000000000, -11.52330688609011844 ) ) ;
#12910 = ORIENTED_EDGE ( 'NONE', *, *, #6353, .T. ) ;
#12911 = ORIENTED_EDGE ( 'NONE', *, *, #7355, .F. ) ;
#12912 = EDGE_CURVE ( 'NONE', #479, #6815, #8660, .T. ) ;
#12913 = ORIENTED_EDGE ( 'NONE', *, *, #6838, .F. ) ;
#12914 = DIRECTION ( 'NONE',  ( 0.000000000000000000, 0.000000000000000000, -1.000000000000000000 ) ) ;
#12915 = LINE ( 'NONE', #12974, #334 ) ;
#12916 = EDGE_CURVE ( 'NONE', #1383, #11595, #944, .T. ) ;
#12917 = CARTESIAN_POINT ( 'NONE',  ( -7.363095878837111030, 9.000000000000000000, 0.009895496992605581216 ) ) ;
#12918 = CARTESIAN_POINT ( 'NONE',  ( 9.250000000000003553, 2.750000000000000888, -10.00000000000000355 ) ) ;
#12919 = CARTESIAN_POINT ( 'NONE',  ( -11.13895890373326836, 0.000000000000000000, 7.723663868796768028 ) ) ;
#12920 = CARTESIAN_POINT ( 'NONE',  ( 2.264806262022877714, 3.000000000000000000, -14.82803603298501471 ) ) ;
#12921 = ORIENTED_EDGE ( 'NONE', *, *, #5705, .T. ) ;
#12922 = EDGE_LOOP ( 'NONE', ( #2505, #7928, #10253, #13224 ) ) ;
#12923 = ADVANCED_FACE ( 'NONE', ( #8163 ), #5661, .F. ) ;
#12924 = CARTESIAN_POINT ( 'NONE',  ( 0.000000000000000000, 0.000000000000000000, -6.750000000000000888 ) ) ;
#12925 = EDGE_CURVE ( 'NONE', #2380, #8347, #1314, .T. ) ;
#12926 = B_SPLINE_SURFACE_WITH_KNOTS ( 'NONE', 2, 1, ( 
 ( #9231, #10337 ),
 ( #8270, #6339 ),
 ( #2079, #3997 ) ),
 .UNSPECIFIED., .F., .F., .F.,
 ( 3, 3 ),
 ( 2, 2 ),
 ( 0.000000000000000000, 1.000000000000000000 ),
 ( 0.000000000000000000, 1.000000000000000000 ),
 .UNSPECIFIED. ) ;
#12927 = VERTEX_POINT ( 'NONE', #12990 ) ;
#12928 = CARTESIAN_POINT ( 'NONE',  ( -12.68816982652970893, 0.000000000000000000, 2.830255545554337004 ) ) ;
#12929 = CARTESIAN_POINT ( 'NONE',  ( 7.723663868796767140, 3.000000000000000000, 11.13895890373327191 ) ) ;
#12930 = CARTESIAN_POINT ( 'NONE',  ( -18.21140389626389222, 0.000000000000000000, 12.49772878833446299 ) ) ;
#12931 = CARTESIAN_POINT ( 'NONE',  ( 8.158551673544282679, 3.000000000000000000, -8.922226997226884393 ) ) ;
#12932 = CARTESIAN_POINT ( 'NONE',  ( -11.63517940784383775, 3.000000000000000000, -7.494008246337203083 ) ) ;
#12933 = DIRECTION ( 'NONE',  ( 0.000000000000000000, 0.000000000000000000, -1.000000000000000000 ) ) ;
#12934 = DIRECTION ( 'NONE',  ( -0.000000000000000000, -1.000000000000000000, -0.000000000000000000 ) ) ;
#12935 = CARTESIAN_POINT ( 'NONE',  ( 12.46219022525837694, 0.000000000000000000, -4.344528055836598845 ) ) ;
#12936 = VERTEX_POINT ( 'NONE', #12100 ) ;
#12937 = ORIENTED_EDGE ( 'NONE', *, *, #8613, .F. ) ;
#12938 = ADVANCED_FACE ( 'NONE', ( #599 ), #6783, .T. ) ;
#12939 = ORIENTED_EDGE ( 'NONE', *, *, #9261, .T. ) ;
#12940 = VERTEX_POINT ( 'NONE', #4587 ) ;
#12941 = DIRECTION ( 'NONE',  ( 0.000000000000000000, 0.000000000000000000, 1.000000000000000000 ) ) ;
#12942 = ORIENTED_EDGE ( 'NONE', *, *, #108, .F. ) ;
#12943 = CARTESIAN_POINT ( 'NONE',  ( 5.708888906988906164, 0.000000000000000000, -11.46847481510586775 ) ) ;
#12944 = LINE ( 'NONE', #8996, #2652 ) ;
#12945 = CARTESIAN_POINT ( 'NONE',  ( 0.000000000000000000, 9.000000000000000000, 0.000000000000000000 ) ) ;
#12946 = PRODUCT_DEFINITION_SHAPE ( 'NONE', 'NONE',  #13618 ) ;
#12947 = FACE_OUTER_BOUND ( 'NONE', #3797, .T. ) ;
#12948 = DIRECTION ( 'NONE',  ( -0.000000000000000000, -1.000000000000000000, -0.000000000000000000 ) ) ;
#12949 = EDGE_CURVE ( 'NONE', #1736, #180, #12176, .T. ) ;
#12950 = ORIENTED_EDGE ( 'NONE', *, *, #6482, .T. ) ;
#12951 = PRESENTATION_STYLE_ASSIGNMENT (( #4347 ) ) ;
#12952 = ORIENTED_EDGE ( 'NONE', *, *, #6794, .T. ) ;
#12953 = B_SPLINE_CURVE_WITH_KNOTS ( 'NONE', 3,
 ( #9021, #10065, #13032, #635 ),
 .UNSPECIFIED., .F., .F.,
 ( 4, 4 ),
 ( 0.1276832474596256706, 1.000000000000000000 ),
 .UNSPECIFIED. ) ;
#12954 = ORIENTED_EDGE ( 'NONE', *, *, #5411, .F. ) ;
#12955 = CARTESIAN_POINT ( 'NONE',  ( -12.98835496148299207, 3.000000000000000000, 0.5501230721524460465 ) ) ;
#12956 = ORIENTED_EDGE ( 'NONE', *, *, #2793, .F. ) ;
#12957 = ORIENTED_EDGE ( 'NONE', *, *, #7184, .T. ) ;
#12958 = DIRECTION ( 'NONE',  ( 0.000000000000000000, 0.000000000000000000, 1.000000000000000000 ) ) ;
#12959 = SHAPE_REPRESENTATION_RELATIONSHIP ( 'NONE' , 'NONE' ,  #11353, #3745 ) ;
#12960 = LINE ( 'NONE', #12701, #5548 ) ;
#12961 = CARTESIAN_POINT ( 'NONE',  ( 24.82664254338761722, 0.000000000000000000, 4.561072489069574409 ) ) ;
#12962 = DIRECTION ( 'NONE',  ( -0.000000000000000000, -1.000000000000000000, -0.000000000000000000 ) ) ;
#12963 = FACE_OUTER_BOUND ( 'NONE', #3296, .T. ) ;
#12964 = CARTESIAN_POINT ( 'NONE',  ( -3.893011711613112880, 3.000000000000000000, -12.40340517008282717 ) ) ;
#12965 = ADVANCED_FACE ( 'NONE', ( #10923 ), #530, .F. ) ;
#12966 = ORIENTED_EDGE ( 'NONE', *, *, #9490, .F. ) ;
#12967 = ADVANCED_FACE ( 'NONE', ( #660 ), #5827, .F. ) ;
#12968 = CARTESIAN_POINT ( 'NONE',  ( 0.000000000000000000, 0.000000000000000000, 0.000000000000000000 ) ) ;
#12969 = ORIENTED_EDGE ( 'NONE', *, *, #1555, .T. ) ;
#12970 = ORIENTED_EDGE ( 'NONE', *, *, #3064, .T. ) ;
#12971 = ORIENTED_EDGE ( 'NONE', *, *, #3714, .F. ) ;
#12972 = AXIS2_PLACEMENT_3D ( 'NONE', #10738, #2134, #211 ) ;
#12973 = CARTESIAN_POINT ( 'NONE',  ( 5.985774866078160450, 9.000000000000000000, 3.119775513178307147 ) ) ;
#12974 = CARTESIAN_POINT ( 'NONE',  ( -14.08504230442587790, 3.000000000000000000, -2.161962830978695571 ) ) ;
#12975 = CARTESIAN_POINT ( 'NONE',  ( 11.14709020439929787, 3.000000000000000000, 7.712570079660892475 ) ) ;
#12976 = B_SPLINE_CURVE_WITH_KNOTS ( 'NONE', 3,
 ( #10866, #4254, #1356, #2251 ),
 .UNSPECIFIED., .F., .F.,
 ( 4, 4 ),
 ( 0.000000000000000000, 0.5855695330273008592 ),
 .UNSPECIFIED. ) ;
#12977 = ADVANCED_FACE ( 'NONE', ( #8772 ), #6540, .F. ) ;
#12978 = CARTESIAN_POINT ( 'NONE',  ( 5.452638258930520010, 3.000000000000000000, -13.97385902380752754 ) ) ;
#12979 = DIRECTION ( 'NONE',  ( -0.000000000000000000, -1.000000000000000000, -0.000000000000000000 ) ) ;
#12980 = DIRECTION ( 'NONE',  ( 0.000000000000000000, 0.000000000000000000, 1.000000000000000000 ) ) ;
#12981 = AXIS2_PLACEMENT_3D ( 'NONE', #13258, #2637, #6844 ) ;
#12982 = VECTOR ( 'NONE', #5217, 1000.000000000000000 ) ;
#12983 = VERTEX_POINT ( 'NONE', #2523 ) ;
#12984 = ADVANCED_FACE ( 'NONE', ( #5619 ), #4652, .F. ) ;
#12985 = ORIENTED_EDGE ( 'NONE', *, *, #12078, .F. ) ;
#12986 = EDGE_CURVE ( 'NONE', #8240, #4834, #4713, .T. ) ;
#12987 = DIRECTION ( 'NONE',  ( -0.000000000000000000, -1.000000000000000000, -0.000000000000000000 ) ) ;
#12988 = ORIENTED_EDGE ( 'NONE', *, *, #12822, .T. ) ;
#12989 = LINE ( 'NONE', #4727, #11297 ) ;
#12990 = CARTESIAN_POINT ( 'NONE',  ( 5.280889752749253319, 9.000000000000000000, -6.660495733750448011 ) ) ;
#12991 = CIRCLE ( 'NONE', #1114, 14.24999999999999822 ) ;
#12992 = AXIS2_PLACEMENT_3D ( 'NONE', #105, #3246, #10633 ) ;
#12993 = DIRECTION ( 'NONE',  ( 0.000000000000000000, 0.000000000000000000, -1.000000000000000000 ) ) ;
#12994 = EDGE_CURVE ( 'NONE', #12802, #710, #1643, .T. ) ;
#12995 = CARTESIAN_POINT ( 'NONE',  ( 3.818534268238711338, 9.000000000000000000, -5.566084444408533116 ) ) ;
#12996 = CARTESIAN_POINT ( 'NONE',  ( -0.7901945867173586491, 3.000000000000000000, -12.78643498603818074 ) ) ;
#12997 = CARTESIAN_POINT ( 'NONE',  ( 20.00000000000000355, 3.000000000000000000, -14.92471123914604370 ) ) ;
#12998 = CARTESIAN_POINT ( 'NONE',  ( 22.00000000000000000, 3.000000000000000000, 1.500000000000000666 ) ) ;
#12999 = DIRECTION ( 'NONE',  ( 0.000000000000000000, 0.000000000000000000, -1.000000000000000000 ) ) ;
#13000 = ORIENTED_EDGE ( 'NONE', *, *, #1948, .T. ) ;
#13001 = VECTOR ( 'NONE', #1416, 1000.000000000000000 ) ;
#13002 = EDGE_LOOP ( 'NONE', ( #4534, #1361, #6137, #3251 ) ) ;
#13003 = VECTOR ( 'NONE', #7486, 1000.000000000000000 ) ;
#13004 = ORIENTED_EDGE ( 'NONE', *, *, #12015, .F. ) ;
#13005 = VERTEX_POINT ( 'NONE', #9950 ) ;
#13006 = CARTESIAN_POINT ( 'NONE',  ( 8.922226997226882617, 0.000000000000000000, 8.158551673544282679 ) ) ;
#13007 = EDGE_LOOP ( 'NONE', ( #2175, #2821, #3580, #1520 ) ) ;
#13008 = CARTESIAN_POINT ( 'NONE',  ( 5.571313494980132397, 0.000000000000000000, -10.72979803820131472 ) ) ;
#13009 =( LENGTH_UNIT ( ) NAMED_UNIT ( * ) SI_UNIT ( .MILLI., .METRE. ) );
#13010 = AXIS2_PLACEMENT_3D ( 'NONE', #1740, #13169, #6973 ) ;
#13011 = ADVANCED_FACE ( 'NONE', ( #13062 ), #3618, .T. ) ;
#13012 = CARTESIAN_POINT ( 'NONE',  ( 26.30958424017656938, 0.09999999999999982514, -4.500000000000000888 ) ) ;
#13013 = CARTESIAN_POINT ( 'NONE',  ( 5.708888906988906164, 3.000000000000000000, -11.46847481510586775 ) ) ;
#13014 = FACE_OUTER_BOUND ( 'NONE', #5781, .T. ) ;
#13015 = CARTESIAN_POINT ( 'NONE',  ( -10.98198414889942676, 3.000000000000000000, -9.379342464487661957 ) ) ;
#13016 = ORIENTED_EDGE ( 'NONE', *, *, #5988, .T. ) ;
#13017 = CARTESIAN_POINT ( 'NONE',  ( 31.00000000000000000, 3.000000000000000000, -1.500000000000003997 ) ) ;
#13018 = EDGE_LOOP ( 'NONE', ( #10934, #1762, #2412, #1837 ) ) ;
#13019 = CLOSED_SHELL ( 'NONE', ( #1465, #10514, #7700, #1629, #3098, #11976, #9380, #3824, #6663, #6665, #2908, #1080, #11935, #1503, #13584, #1303, #10177, #7437, #2530, #133, #8593, #12156, #11138, #1881, #13151, #4978, #12967, #3059, #13543, #4082, #9396, #12421, #5063, #3683, #13489, #8183, #3733, #3613, #7825, #111, #6924, #12772, #3544, #1403, #118 ) ) ;
#13020 = ORIENTED_EDGE ( 'NONE', *, *, #208, .F. ) ;
#13021 = CARTESIAN_POINT ( 'NONE',  ( 19.60942157306000766, 3.000000000000000000, 14.05941790610251374 ) ) ;
#13022 = DIRECTION ( 'NONE',  ( -0.000000000000000000, -1.000000000000000000, -0.000000000000000000 ) ) ;
#13023 = CIRCLE ( 'NONE', #9058, 1.500000000000000222 ) ;
#13024 = VERTEX_POINT ( 'NONE', #13129 ) ;
#13025 = EDGE_LOOP ( 'NONE', ( #240, #425 ) ) ;
#13026 = CARTESIAN_POINT ( 'NONE',  ( 0.000000000000000000, 0.000000000000000000, 0.000000000000000000 ) ) ;
#13027 = DIRECTION ( 'NONE',  ( 0.000000000000000000, 0.000000000000000000, -1.000000000000000000 ) ) ;
#13028 = CARTESIAN_POINT ( 'NONE',  ( 30.79170750349150509, 0.000000000000000000, -0.0004760053210284623249 ) ) ;
#13029 = VECTOR ( 'NONE', #2611, 1000.000000000000000 ) ;
#13030 = CARTESIAN_POINT ( 'NONE',  ( 9.325031192972383920, 0.000000000000000000, -9.065266643391169055 ) ) ;
#13031 = VECTOR ( 'NONE', #11024, 1000.000000000000000 ) ;
#13032 = CARTESIAN_POINT ( 'NONE',  ( -0.8776997859584816375, 0.000000000000000000, 7.310603390113379341 ) ) ;
#13033 = CARTESIAN_POINT ( 'NONE',  ( -0.8123631076467130452, 9.000000000000000000, -6.700937709107179785 ) ) ;
#13034 = ORIENTED_EDGE ( 'NONE', *, *, #10547, .F. ) ;
#13035 = DIRECTION ( 'NONE',  ( -0.000000000000000000, -1.000000000000000000, -0.000000000000000000 ) ) ;
#13036 = B_SPLINE_SURFACE_WITH_KNOTS ( 'NONE', 2, 1, ( 
 ( #11269, #3892 ),
 ( #1916, #2794 ),
 ( #3958, #7003 ) ),
 .UNSPECIFIED., .F., .F., .F.,
 ( 3, 3 ),
 ( 2, 2 ),
 ( 0.000000000000000000, 1.000000000000000000 ),
 ( 0.000000000000000000, 1.000000000000000000 ),
 .UNSPECIFIED. ) ;
#13037 = ORIENTED_EDGE ( 'NONE', *, *, #3893, .F. ) ;
#13038 = ORIENTED_EDGE ( 'NONE', *, *, #8339, .T. ) ;
#13039 = ORIENTED_EDGE ( 'NONE', *, *, #8254, .F. ) ;
#13040 = AXIS2_PLACEMENT_3D ( 'NONE', #1935, #4188, #9372 ) ;
#13041 = AXIS2_PLACEMENT_3D ( 'NONE', #4524, #9819, #392 ) ;
#13042 = VECTOR ( 'NONE', #10233, 1000.000000000000000 ) ;
#13043 = EDGE_CURVE ( 'NONE', #344, #10535, #5158, .T. ) ;
#13044 = DIRECTION ( 'NONE',  ( -0.000000000000000000, -1.000000000000000000, 0.000000000000000000 ) ) ;
#13045 = CARTESIAN_POINT ( 'NONE',  ( -13.49999999999999645, 0.000000000000000000, -7.049999999999998934 ) ) ;
#13046 = CARTESIAN_POINT ( 'NONE',  ( 6.530577460941774603, 0.000000000000000000, 3.402183248810843885 ) ) ;
#13047 = DIRECTION ( 'NONE',  ( 0.000000000000000000, 0.000000000000000000, 1.000000000000000000 ) ) ;
#13048 = ITEM_DEFINED_TRANSFORMATION ( 'NONE', 'NONE', #805,  #10007 ) ;
#13049 = CARTESIAN_POINT ( 'NONE',  ( -7.363095878837111030, 0.000000000000000000, 0.009895496992605581216 ) ) ;
#13050 = CARTESIAN_POINT ( 'NONE',  ( 9.379342464487701037, 0.000000000000000000, -10.98198414889939301 ) ) ;
#13051 = DIRECTION ( 'NONE',  ( 0.000000000000000000, 1.000000000000000000, -0.000000000000000000 ) ) ;
#13052 = CARTESIAN_POINT ( 'NONE',  ( 0.8327827707325454742, 0.000000000000000000, 6.698430626405788679 ) ) ;
#13053 = CIRCLE ( 'NONE', #13285, 13.50000000000000178 ) ;
#13054 = CIRCLE ( 'NONE', #11728, 1.499999999686092877 ) ;
#13055 = ORIENTED_EDGE ( 'NONE', *, *, #6999, .T. ) ;
#13056 = ORIENTED_EDGE ( 'NONE', *, *, #5633, .T. ) ;
#13057 = EDGE_CURVE ( 'NONE', #5187, #9552, #4584, .T. ) ;
#13058 = ORIENTED_EDGE ( 'NONE', *, *, #3579, .F. ) ;
#13059 = FACE_OUTER_BOUND ( 'NONE', #11193, .T. ) ;
#13060 = VECTOR ( 'NONE', #8555, 1000.000000000000000 ) ;
#13061 = AXIS2_PLACEMENT_3D ( 'NONE', #9166, #5032, #4196 ) ;
#13062 = FACE_OUTER_BOUND ( 'NONE', #482, .T. ) ;
#13063 = EDGE_CURVE ( 'NONE', #12786, #6748, #6914, .T. ) ;
#13064 = DIRECTION ( 'NONE',  ( -0.000000000000000000, -1.000000000000000000, -0.000000000000000000 ) ) ;
#13065 = ADVANCED_FACE ( 'NONE', ( #9051 ), #5136, .T. ) ;
#13066 = FACE_OUTER_BOUND ( 'NONE', #7651, .T. ) ;
#13067 = CARTESIAN_POINT ( 'NONE',  ( 31.00000000000000000, 0.000000000000000000, -3.399999999999999911 ) ) ;
#13068 = CARTESIAN_POINT ( 'NONE',  ( -10.97318381393799136, 0.000000000000000000, -6.970598036433411693 ) ) ;
#13069 = DIRECTION ( 'NONE',  ( 0.000000000000000000, 0.000000000000000000, -1.000000000000000000 ) ) ;
#13070 = AXIS2_PLACEMENT_3D ( 'NONE', #10034, #4798, #9959 ) ;
#13071 = CARTESIAN_POINT ( 'NONE',  ( -13.97385902380755240, 3.000000000000000000, -5.452638258930474713 ) ) ;
#13072 = AXIS2_PLACEMENT_3D ( 'NONE', #13363, #8115, #10466 ) ;
#13073 = ORIENTED_EDGE ( 'NONE', *, *, #7184, .F. ) ;
#13074 = EDGE_LOOP ( 'NONE', ( #4669, #6275, #6576, #10343 ) ) ;
#13075 = AXIS2_PLACEMENT_3D ( 'NONE', #13176, #9804, #10075 ) ;
#13076 = ORIENTED_EDGE ( 'NONE', *, *, #3217, .F. ) ;
#13077 = ORIENTED_EDGE ( 'NONE', *, *, #11475, .T. ) ;
#13078 = DIRECTION ( 'NONE',  ( -3.061616997868383141E-16, 0.000000000000000000, -1.000000000000000000 ) ) ;
#13079 = EDGE_CURVE ( 'NONE', #13528, #11718, #1412, .T. ) ;
#13080 = ORIENTED_EDGE ( 'NONE', *, *, #12986, .T. ) ;
#13081 = LINE ( 'NONE', #9970, #4385 ) ;
#13082 = SURFACE_STYLE_USAGE ( .BOTH. , #3361 ) ;
#13083 = EDGE_CURVE ( 'NONE', #2891, #6390, #2298, .T. ) ;
#13084 = DIRECTION ( 'NONE',  ( 0.000000000000000000, 0.000000000000000000, -1.000000000000000000 ) ) ;
#13085 = DIRECTION ( 'NONE',  ( 0.000000000000000000, 0.000000000000000000, 1.000000000000000000 ) ) ;
#13086 = CIRCLE ( 'NONE', #8676, 1.500000000000001332 ) ;
#13087 = CARTESIAN_POINT ( 'NONE',  ( -5.733772933379540859, 3.000000000000000000, -13.04554897075796660 ) ) ;
#13088 = DIRECTION ( 'NONE',  ( 0.000000000000000000, 1.000000000000000000, -0.000000000000000000 ) ) ;
#13089 = DIRECTION ( 'NONE',  ( 0.000000000000000000, 0.000000000000000000, -1.000000000000000000 ) ) ;
#13090 = ORIENTED_EDGE ( 'NONE', *, *, #3550, .T. ) ;
#13091 = DIRECTION ( 'NONE',  ( 0.000000000000000000, 0.000000000000000000, -1.000000000000000000 ) ) ;
#13092 = ORIENTED_EDGE ( 'NONE', *, *, #10030, .F. ) ;
#13093 = ORIENTED_EDGE ( 'NONE', *, *, #362, .T. ) ;
#13094 = CIRCLE ( 'NONE', #12884, 1.500000000000001332 ) ;
#13095 = CARTESIAN_POINT ( 'NONE',  ( 1.650143266773734796, 3.000000000000000000, -14.90895795148410841 ) ) ;
#13096 = EDGE_CURVE ( 'NONE', #7606, #13159, #12250, .T. ) ;
#13097 = EDGE_CURVE ( 'NONE', #11231, #2693, #6253, .T. ) ;
#13098 = VERTEX_POINT ( 'NONE', #11198 ) ;
#13099 = MANIFOLD_SOLID_BREP ( 'Boss-Extrude1', #13250 ) ;
#13100 = ORIENTED_EDGE ( 'NONE', *, *, #10073, .T. ) ;
#13101 = CARTESIAN_POINT ( 'NONE',  ( 0.8653219153705552502, 9.000000000000000000, -7.312626806738413698 ) ) ;
#13102 =( NAMED_UNIT ( * ) PLANE_ANGLE_UNIT ( ) SI_UNIT ( $, .RADIAN. ) );
#13103 = CARTESIAN_POINT ( 'NONE',  ( -6.515098946627274401, -1.694065894508600678E-18, 3.430563300314522390 ) ) ;
#13104 = CARTESIAN_POINT ( 'NONE',  ( -12.40347894490204972, 0.000000000000000000, 3.892776652129660064 ) ) ;
#13105 = DIRECTION ( 'NONE',  ( 0.000000000000000000, 0.000000000000000000, 1.000000000000000000 ) ) ;
#13106 = DIRECTION ( 'NONE',  ( 0.000000000000000000, 0.000000000000000000, -1.000000000000000000 ) ) ;
#13107 = ORIENTED_EDGE ( 'NONE', *, *, #12277, .F. ) ;
#13108 = CARTESIAN_POINT ( 'NONE',  ( 3.647599401157688437, 3.000000000000000000, 11.52662650599083882 ) ) ;
#13109 = ORIENTED_EDGE ( 'NONE', *, *, #6647, .F. ) ;
#13110 = ORIENTED_EDGE ( 'NONE', *, *, #678, .F. ) ;
#13111 = EDGE_LOOP ( 'NONE', ( #4553, #625, #8400, #12609 ) ) ;
#13112 = PRODUCT_DEFINITION_FORMATION_WITH_SPECIFIED_SOURCE ( 'ANY', '', #8958, .NOT_KNOWN. ) ;
#13113 = DIRECTION ( 'NONE',  ( 0.000000000000000000, 1.000000000000000000, -0.000000000000000000 ) ) ;
#13114 = CARTESIAN_POINT ( 'NONE',  ( 30.79786191028635400, 3.000000000000000000, -7.999232361977356653 ) ) ;
#13115 = DIRECTION ( 'NONE',  ( 0.000000000000000000, 1.000000000000000000, 0.000000000000000000 ) ) ;
#13116 = CARTESIAN_POINT ( 'NONE',  ( 0.000000000000000000, 0.09999999999999982514, 0.000000000000000000 ) ) ;
#13117 = FACE_OUTER_BOUND ( 'NONE', #3505, .T. ) ;
#13118 = CONTEXT_DEPENDENT_SHAPE_REPRESENTATION ( #6258, #3476 ) ;
#13119 = LINE ( 'NONE', #799, #2268 ) ;
#13120 = DIRECTION ( 'NONE',  ( -0.000000000000000000, -1.000000000000000000, 0.000000000000000000 ) ) ;
#13121 = CARTESIAN_POINT ( 'NONE',  ( 4.690415759823430619, 3.000000000000000000, -1.399999999999999911 ) ) ;
#13122 = CARTESIAN_POINT ( 'NONE',  ( -18.21140389626389577, 3.000000000000000000, -14.83930531255816376 ) ) ;
#13123 = DIRECTION ( 'NONE',  ( -0.000000000000000000, -1.000000000000000000, -0.000000000000000000 ) ) ;
#13124 = ORIENTED_EDGE ( 'NONE', *, *, #3526, .T. ) ;
#13125 = EDGE_CURVE ( 'NONE', #9840, #12067, #3891, .T. ) ;
#13126 = ORIENTED_EDGE ( 'NONE', *, *, #8822, .T. ) ;
#13127 = VERTEX_POINT ( 'NONE', #7148 ) ;
#13128 = CARTESIAN_POINT ( 'NONE',  ( 5.733772933379541747, 3.000000000000000000, 13.04554897075796482 ) ) ;
#13129 = CARTESIAN_POINT ( 'NONE',  ( -8.883544964652065445, 0.000000000000000000, -12.08646469655229438 ) ) ;
#13130 = CARTESIAN_POINT ( 'NONE',  ( 54.70014691233865989, 0.000000000000000000, -3.785783530882224746 ) ) ;
#13131 = DIRECTION ( 'NONE',  ( -0.000000000000000000, -1.000000000000000000, -0.000000000000000000 ) ) ;
#13132 = DIRECTION ( 'NONE',  ( -0.000000000000000000, -1.000000000000000000, -0.000000000000000000 ) ) ;
#13133 = CARTESIAN_POINT ( 'NONE',  ( 0.000000000000000000, 0.09999999999999982514, 0.000000000000000000 ) ) ;
#13134 = EDGE_CURVE ( 'NONE', #11941, #9276, #6048, .T. ) ;
#13135 = CARTESIAN_POINT ( 'NONE',  ( 3.893011711613070691, 3.000000000000000000, -12.40340517008307231 ) ) ;
#13136 = EDGE_CURVE ( 'NONE', #9925, #9010, #810, .T. ) ;
#13137 = CARTESIAN_POINT ( 'NONE',  ( 12.01285915242476499, 0.000000000000000000, -4.000000001073668265 ) ) ;
#13138 = VERTEX_POINT ( 'NONE', #12525 ) ;
#13139 = ORIENTED_EDGE ( 'NONE', *, *, #2578, .T. ) ;
#13140 = ORIENTED_EDGE ( 'NONE', *, *, #12852, .T. ) ;
#13141 = FACE_OUTER_BOUND ( 'NONE', #9076, .T. ) ;
#13142 = EDGE_CURVE ( 'NONE', #11521, #7533, #9117, .T. ) ;
#13143 = VERTEX_POINT ( 'NONE', #1973 ) ;
#13144 = CARTESIAN_POINT ( 'NONE',  ( 31.00000000000000000, 2.900000000000000355, 3.399999999999999911 ) ) ;
#13145 = DIRECTION ( 'NONE',  ( -0.5494223406529682441, -2.363163406253605394E-16, 0.8355447873043153617 ) ) ;
#13146 = PRODUCT_DEFINITION_SHAPE ( 'NONE', 'NONE',  #10603 ) ;
#13147 = DIRECTION ( 'NONE',  ( -0.000000000000000000, -1.000000000000000000, -0.000000000000000000 ) ) ;
#13148 = CARTESIAN_POINT ( 'NONE',  ( 0.000000000000000000, 0.000000000000000000, 0.000000000000000000 ) ) ;
#13149 = B_SPLINE_CURVE_WITH_KNOTS ( 'NONE', 3,
 ( #10829, #233, #10636, #1259 ),
 .UNSPECIFIED., .F., .F.,
 ( 4, 4 ),
 ( 0.1547128134717859205, 1.000000000000000000 ),
 .UNSPECIFIED. ) ;
#13150 = DIRECTION ( 'NONE',  ( -0.000000000000000000, -1.000000000000000000, -0.000000000000000000 ) ) ;
#13151 = ADVANCED_FACE ( 'NONE', ( #8230 ), #5061, .F. ) ;
#13152 = CARTESIAN_POINT ( 'NONE',  ( -11.35348746973813761, 0.000000000000000000, -6.343077501554963860 ) ) ;
#13153 = CARTESIAN_POINT ( 'NONE',  ( 2.161962830978677363, 0.000000000000000000, 14.08504230442587613 ) ) ;
#13154 = ORIENTED_EDGE ( 'NONE', *, *, #7193, .T. ) ;
#13155 = SURFACE_STYLE_USAGE ( .BOTH. , #12128 ) ;
#13156 = ORIENTED_EDGE ( 'NONE', *, *, #4144, .T. ) ;
#13157 = UNCERTAINTY_MEASURE_WITH_UNIT (LENGTH_MEASURE( 1.000000000000000082E-05 ), #835, 'distance_accuracy_value', 'NONE');
#13158 = ADVANCED_FACE ( 'NONE', ( #3004 ), #7540, .F. ) ;
#13159 = VERTEX_POINT ( 'NONE', #4163 ) ;
#13160 = CARTESIAN_POINT ( 'NONE',  ( -7.712570079660889810, 3.000000000000000000, 11.14709020439930320 ) ) ;
#13161 = EDGE_CURVE ( 'NONE', #12893, #7299, #1422, .T. ) ;
#13162 = B_SPLINE_CURVE_WITH_KNOTS ( 'NONE', 3,
 ( #9650, #1051, #10625, #12700 ),
 .UNSPECIFIED., .F., .F.,
 ( 4, 4 ),
 ( 0.000000000000000000, 0.5855695330273008592 ),
 .UNSPECIFIED. ) ;
#13163 = ORIENTED_EDGE ( 'NONE', *, *, #8503, .T. ) ;
#13164 = ORIENTED_EDGE ( 'NONE', *, *, #10984, .F. ) ;
#13165 = CARTESIAN_POINT ( 'NONE',  ( -12.30759122141990325, 3.000000000000000000, -6.329356821613475681 ) ) ;
#13166 = LINE ( 'NONE', #12070, #13031 ) ;
#13167 = DIRECTION ( 'NONE',  ( -0.000000000000000000, -1.000000000000000000, -0.000000000000000000 ) ) ;
#13168 = CARTESIAN_POINT ( 'NONE',  ( -5.571433138827826426, 0.000000000000000000, -10.72973591378220526 ) ) ;
#13169 = DIRECTION ( 'NONE',  ( -1.000000000000000000, 3.469446951953610639E-15, 2.602085213965210149E-16 ) ) ;
#13170 = DIRECTION ( 'NONE',  ( -0.000000000000000000, -1.000000000000000000, -0.000000000000000000 ) ) ;
#13171 = ORIENTED_EDGE ( 'NONE', *, *, #7422, .F. ) ;
#13172 = DIRECTION ( 'NONE',  ( 0.000000000000000000, -0.000000000000000000, -1.000000000000000000 ) ) ;
#13173 = ORIENTED_EDGE ( 'NONE', *, *, #2431, .F. ) ;
#13174 = ORIENTED_EDGE ( 'NONE', *, *, #1620, .T. ) ;
#13175 = ORIENTED_EDGE ( 'NONE', *, *, #2823, .F. ) ;
#13176 = CARTESIAN_POINT ( 'NONE',  ( 0.000000000000000000, 0.000000000000000000, 0.000000000000000000 ) ) ;
#13177 = CARTESIAN_POINT ( 'NONE',  ( 4.564691384634508964, 3.000000000000000000, -12.76342233970727413 ) ) ;
#13178 = CARTESIAN_POINT ( 'NONE',  ( 5.170206418547604876, 3.000000000000000000, -13.27898586450069196 ) ) ;
#13179 = CARTESIAN_POINT ( 'NONE',  ( -10.72973591378220348, 3.000000000000000000, 5.571433138827830867 ) ) ;
#13180 = CARTESIAN_POINT ( 'NONE',  ( -12.60833596047604210, 0.000000000000000000, -3.188441730140805674 ) ) ;
#13181 = CARTESIAN_POINT ( 'NONE',  ( -8.914835885878282795, 3.000000000000000000, -11.11702303352191556 ) ) ;
#13182 = ADVANCED_FACE ( 'NONE', ( #8625 ), #499, .F. ) ;
#13183 = DIRECTION ( 'NONE',  ( 0.000000000000000000, 1.000000000000000000, 0.000000000000000000 ) ) ;
#13184 = FACE_BOUND ( 'NONE', #13307, .T. ) ;
#13185 = EDGE_CURVE ( 'NONE', #5359, #8240, #11611, .T. ) ;
#13186 = FACE_OUTER_BOUND ( 'NONE', #268, .T. ) ;
#13187 = LINE ( 'NONE', #1833, #5768 ) ;
#13188 = ORIENTED_EDGE ( 'NONE', *, *, #5333, .T. ) ;
#13189 = EDGE_LOOP ( 'NONE', ( #6550, #4142, #11557, #5228 ) ) ;
#13190 = VECTOR ( 'NONE', #11286, 1000.000000000000000 ) ;
#13191 = ORIENTED_EDGE ( 'NONE', *, *, #10280, .F. ) ;
#13192 = DIRECTION ( 'NONE',  ( -0.000000000000000000, -1.000000000000000000, -0.000000000000000000 ) ) ;
#13193 = CARTESIAN_POINT ( 'NONE',  ( -6.970598036433426792, 3.000000000000000000, -10.97318381393771780 ) ) ;
#13194 = CARTESIAN_POINT ( 'NONE',  ( 12.00000000000001954, 8.000000000000000000, -6.999999999999999112 ) ) ;
#13195 = AXIS2_PLACEMENT_3D ( 'NONE', #4795, #10244, #8981 ) ;
#13196 = DIRECTION ( 'NONE',  ( 0.000000000000000000, 0.000000000000000000, -1.000000000000000000 ) ) ;
#13197 = CYLINDRICAL_SURFACE ( 'NONE', #696, 12.99999999999977973 ) ;
#13198 = AXIS2_PLACEMENT_3D ( 'NONE', #3048, #3109, #5194 ) ;
#13199 = DIRECTION ( 'NONE',  ( -0.000000000000000000, -1.000000000000000000, -0.000000000000000000 ) ) ;
#13200 = FACE_OUTER_BOUND ( 'NONE', #2228, .T. ) ;
#13201 = DIRECTION ( 'NONE',  ( 1.224646799147353454E-16, 0.000000000000000000, -1.000000000000000000 ) ) ;
#13202 = ORIENTED_EDGE ( 'NONE', *, *, #5648, .T. ) ;
#13203 = ORIENTED_EDGE ( 'NONE', *, *, #9512, .T. ) ;
#13204 = ORIENTED_EDGE ( 'NONE', *, *, #10938, .T. ) ;
#13205 = DIRECTION ( 'NONE',  ( 0.000000000000000000, 1.000000000000000000, -0.000000000000000000 ) ) ;
#13206 = VECTOR ( 'NONE', #11124, 1000.000000000000000 ) ;
#13207 = CIRCLE ( 'NONE', #7919, 1.500000000000001332 ) ;
#13208 = EDGE_LOOP ( 'NONE', ( #9940, #1869, #3354, #1461 ) ) ;
#13209 = EDGE_CURVE ( 'NONE', #4927, #12265, #548, .T. ) ;
#13210 = CARTESIAN_POINT ( 'NONE',  ( 0.000000000000000000, 0.000000000000000000, 0.000000000000000000 ) ) ;
#13211 = DIRECTION ( 'NONE',  ( -0.8209917224599529995, -1.537059293307744984E-25, 0.5709400946266076637 ) ) ;
#13212 = LINE ( 'NONE', #1371, #2440 ) ;
#13213 = CARTESIAN_POINT ( 'NONE',  ( -0.8973464813148227526, -1.694065894508600678E-18, -7.308217849399443189 ) ) ;
#13214 = PLANE ( 'NONE',  #115 ) ;
#13215 = VECTOR ( 'NONE', #1353, 1000.000000000000000 ) ;
#13216 = CARTESIAN_POINT ( 'NONE',  ( 0.000000000000000000, 0.000000000000000000, 0.000000000000000000 ) ) ;
#13217 = TOROIDAL_SURFACE ( 'NONE', #4195, 3.100000000000000977, 0.1000000000000000056 ) ;
#13218 = DIRECTION ( 'NONE',  ( -0.000000000000000000, -1.000000000000000000, -0.000000000000000000 ) ) ;
#13219 = VERTEX_POINT ( 'NONE', #4304 ) ;
#13220 = CARTESIAN_POINT ( 'NONE',  ( -5.733772933379541747, 3.000000000000000000, -13.04554897075796482 ) ) ;
#13221 = EDGE_LOOP ( 'NONE', ( #486, #3706, #6344, #5875 ) ) ;
#13222 = ORIENTED_EDGE ( 'NONE', *, *, #9540, .F. ) ;
#13223 = CARTESIAN_POINT ( 'NONE',  ( -2.976187484161006314, 9.000000000000000000, 7.363908159724035229 ) ) ;
#13224 = ORIENTED_EDGE ( 'NONE', *, *, #7510, .F. ) ;
#13225 = LINE ( 'NONE', #5921, #8208 ) ;
#13227 = MANIFOLD_SOLID_BREP ( 'Fillet1', #7733 ) ;
#13226 = VECTOR ( 'NONE', #5949, 1000.000000000000000 ) ;
#13228 = VERTEX_POINT ( 'NONE', #11548 ) ;
#13229 = AXIS2_PLACEMENT_3D ( 'NONE', #7543, #9409, #10578 ) ;
#13230 = EDGE_CURVE ( 'NONE', #12683, #10097, #996, .T. ) ;
#13231 = DIRECTION ( 'NONE',  ( -0.000000000000000000, -1.000000000000000000, -0.000000000000000000 ) ) ;
#13232 =( NAMED_UNIT ( * ) SI_UNIT ( $, .STERADIAN. ) SOLID_ANGLE_UNIT ( ) );
#13233 = CARTESIAN_POINT ( 'NONE',  ( -6.329356821613726147, 0.000000000000000000, -12.30759122142001338 ) ) ;
#13234 = CARTESIAN_POINT ( 'NONE',  ( 1.557181465540758758, 0.000000000000000000, 14.16466328168009881 ) ) ;
#13235 = EDGE_CURVE ( 'NONE', #9925, #4390, #12651, .T. ) ;
#13236 = CARTESIAN_POINT ( 'NONE',  ( 11.48836750521724070, 0.000000000000000000, 8.430890348300627224 ) ) ;
#13237 = ADVANCED_FACE ( 'NONE', ( #8494 ), #3257, .T. ) ;
#13238 = LINE ( 'NONE', #12142, #5977 ) ;
#13239 = DIRECTION ( 'NONE',  ( 0.7842105416216805791, -0.000000000000000000, 0.6204948238377419045 ) ) ;
#13240 = ORIENTED_EDGE ( 'NONE', *, *, #4313, .T. ) ;
#13241 = CARTESIAN_POINT ( 'NONE',  ( -6.017756925049793537, 0.000000000000000000, -11.52330688609026232 ) ) ;
#13242 = CIRCLE ( 'NONE', #13010, 0.7499999999999997780 ) ;
#13243 = EDGE_LOOP ( 'NONE', ( #6884, #4409, #377, #3015 ) ) ;
#13244 = VERTEX_POINT ( 'NONE', #9605 ) ;
#13245 = CARTESIAN_POINT ( 'NONE',  ( 54.70014691233865989, 3.000000000000000000, -3.785783530882224746 ) ) ;
#13246 = B_SPLINE_CURVE_WITH_KNOTS ( 'NONE', 3,
 ( #10393, #5090, #5023, #12484 ),
 .UNSPECIFIED., .F., .F.,
 ( 4, 4 ),
 ( 0.1547128134717859205, 1.000000000000000000 ),
 .UNSPECIFIED. ) ;
#13247 = ORIENTED_EDGE ( 'NONE', *, *, #7014, .T. ) ;
#13248 = EDGE_CURVE ( 'NONE', #2012, #8754, #985, .T. ) ;
#13249 = CYLINDRICAL_SURFACE ( 'NONE', #5746, 0.1000000000000000472 ) ;
#13250 = CLOSED_SHELL ( 'NONE', ( #6000, #10575, #6392, #13523, #3120, #8202, #12984, #8097, #6413, #6324, #4501, #10296, #8416, #4430, #11896, #12575, #5403, #9697, #9111, #9607, #10815, #12271, #12881, #250, #6248, #9938, #12965, #12527, #1297, #12239, #8961, #10455, #5344 ) ) ;
#13251 = CARTESIAN_POINT ( 'NONE',  ( 11.11702303352191912, 0.000000000000000000, -8.914835885878277466 ) ) ;
#13252 = CIRCLE ( 'NONE', #7312, 0.7500000000000024425 ) ;
#13253 = CARTESIAN_POINT ( 'NONE',  ( -7.500000000000000000, 0.000000000000000000, 0.000000000000000000 ) ) ;
#13254 = CARTESIAN_POINT ( 'NONE',  ( -13.00394572736061605, 0.000000000000000000, 0.1835083749157108701 ) ) ;
#13255 = CARTESIAN_POINT ( 'NONE',  ( -5.299649803506882861, 9.000000000000000000, -6.645578376649353913 ) ) ;
#13256 = FACE_OUTER_BOUND ( 'NONE', #8395, .T. ) ;
#13257 = EDGE_CURVE ( 'NONE', #5342, #8278, #7228, .T. ) ;
#13258 = CARTESIAN_POINT ( 'NONE',  ( 2.453448243599948952, 2.900000000000000355, -2.353846153846153921 ) ) ;
#13259 = CARTESIAN_POINT ( 'NONE',  ( 0.000000000000000000, 0.000000000000000000, 0.000000000000000000 ) ) ;
#13260 = CYLINDRICAL_SURFACE ( 'NONE', #9315, 13.50000000000000178 ) ;
#13261 = CARTESIAN_POINT ( 'NONE',  ( 0.000000000000000000, 3.000000000000000000, 0.000000000000000000 ) ) ;
#13262 = ORIENTED_EDGE ( 'NONE', *, *, #2334, .T. ) ;
#13263 = ORIENTED_EDGE ( 'NONE', *, *, #5046, .T. ) ;
#13264 = AXIS2_PLACEMENT_3D ( 'NONE', #7595, #1254, #8542 ) ;
#13265 = AXIS2_PLACEMENT_3D ( 'NONE', #6922, #4992, #11050 ) ;
#13266 = EDGE_CURVE ( 'NONE', #7204, #2253, #4434, .T. ) ;
#13267 = EDGE_CURVE ( 'NONE', #8960, #3116, #165, .T. ) ;
#13268 = VERTEX_POINT ( 'NONE', #8818 ) ;
#13269 = CARTESIAN_POINT ( 'NONE',  ( 2.720000000000001528, 2.000000000000000000, 4.500000000000000000 ) ) ;
#13270 = CARTESIAN_POINT ( 'NONE',  ( 8.180229652970799847, 0.000000000000000000, -11.90209577080762848 ) ) ;
#13271 = AXIS2_PLACEMENT_3D ( 'NONE', #1295, #148, #11840 ) ;
#13272 = CARTESIAN_POINT ( 'NONE',  ( -13.28140389626389783, 0.000000000000000000, 13.39999999999999858 ) ) ;
#13273 = AXIS2_PLACEMENT_3D ( 'NONE', #124, #2107, #6437 ) ;
#13274 = EDGE_CURVE ( 'NONE', #11577, #1280, #8672, .T. ) ;
#13275 = CARTESIAN_POINT ( 'NONE',  ( 26.30958424017656938, 2.900000000000000355, 4.500000000000000888 ) ) ;
#13276 = DIRECTION ( 'NONE',  ( 0.000000000000000000, 0.000000000000000000, -1.000000000000000000 ) ) ;
#13277 = DIRECTION ( 'NONE',  ( 0.000000000000000000, 0.000000000000000000, 1.000000000000000000 ) ) ;
#13278 = CARTESIAN_POINT ( 'NONE',  ( 11.65525440103098731, 3.000000000000000000, 2.142386537870793362 ) ) ;
#13279 = CARTESIAN_POINT ( 'NONE',  ( -0.5398653231797316820, 0.000000000000000000, 12.07794044664754018 ) ) ;
#13280 = ORIENTED_EDGE ( 'NONE', *, *, #12912, .T. ) ;
#13281 = ORIENTED_EDGE ( 'NONE', *, *, #5409, .F. ) ;
#13282 = ORIENTED_EDGE ( 'NONE', *, *, #12088, .F. ) ;
#13283 = CIRCLE ( 'NONE', #8639, 0.09999999999999982514 ) ;
#13284 = DIRECTION ( 'NONE',  ( 0.000000000000000000, 1.000000000000000000, -0.000000000000000000 ) ) ;
#13285 = AXIS2_PLACEMENT_3D ( 'NONE', #8145, #4843, #1755 ) ;
#13286 = CIRCLE ( 'NONE', #7537, 8.500000000000001776 ) ;
#13287 = ORIENTED_EDGE ( 'NONE', *, *, #4427, .F. ) ;
#13288 = LINE ( 'NONE', #10254, #9221 ) ;
#13289 = DIRECTION ( 'NONE',  ( -0.9353363873783847593, -6.543406766095367948E-22, 0.3537595828326807190 ) ) ;
#13290 = DIRECTION ( 'NONE',  ( 0.000000000000000000, 0.000000000000000000, 1.000000000000000000 ) ) ;
#13291 = DIRECTION ( 'NONE',  ( -0.000000000000000000, -1.000000000000000000, -0.000000000000000000 ) ) ;
#13292 = CARTESIAN_POINT ( 'NONE',  ( 0.000000000000000000, 3.000000000000000000, -12.08999999999737440 ) ) ;
#13293 = AXIS2_PLACEMENT_3D ( 'NONE', #2077, #10481, #839 ) ;
#13294 = DIRECTION ( 'NONE',  ( 0.000000000000000000, 0.000000000000000000, -1.000000000000000000 ) ) ;
#13295 = CARTESIAN_POINT ( 'NONE',  ( -12.98835496148321944, 3.000000000000000000, -0.5501230721522551992 ) ) ;
#13296 = ORIENTED_EDGE ( 'NONE', *, *, #4762, .F. ) ;
#13297 =( LENGTH_UNIT ( ) NAMED_UNIT ( * ) SI_UNIT ( .MILLI., .METRE. ) );
#13298 = VERTEX_POINT ( 'NONE', #10910 ) ;
#13299 = UNCERTAINTY_MEASURE_WITH_UNIT (LENGTH_MEASURE( 1.000000000000000082E-05 ), #10404, 'distance_accuracy_value', 'NONE');
#13300 = EDGE_CURVE ( 'NONE', #8949, #4662, #7863, .T. ) ;
#13301 = ORIENTED_EDGE ( 'NONE', *, *, #864, .T. ) ;
#13302 = DIRECTION ( 'NONE',  ( 0.000000000000000000, 0.000000000000000000, 1.000000000000000000 ) ) ;
#13303 = ORIENTED_EDGE ( 'NONE', *, *, #3026, .F. ) ;
#13304 = VECTOR ( 'NONE', #5528, 1000.000000000000000 ) ;
#13305 = CARTESIAN_POINT ( 'NONE',  ( 2.830255545554135832, 0.000000000000000000, -12.68816982652952596 ) ) ;
#13306 = VECTOR ( 'NONE', #6801, 1000.000000000000000 ) ;
#13307 = EDGE_LOOP ( 'NONE', ( #361, #13037 ) ) ;
#13308 = AXIS2_PLACEMENT_3D ( 'NONE', #8603, #8477, #4207 ) ;
#13309 = DIRECTION ( 'NONE',  ( 0.000000000000000000, 0.000000000000000000, -1.000000000000000000 ) ) ;
#13310 = FILL_AREA_STYLE_COLOUR ( '', #6707 ) ;
#13311 = DIRECTION ( 'NONE',  ( 0.000000000000000000, 0.000000000000000000, -1.000000000000000000 ) ) ;
#13312 = CARTESIAN_POINT ( 'NONE',  ( -2.976187484161006314, 0.000000000000000000, 7.363908159724035229 ) ) ;
#13313 = DIRECTION ( 'NONE',  ( 0.000000000000000000, 0.000000000000000000, 1.000000000000000000 ) ) ;
#13314 = DIRECTION ( 'NONE',  ( -0.000000000000000000, -1.000000000000000000, -0.000000000000000000 ) ) ;
#13315 = CARTESIAN_POINT ( 'NONE',  ( 9.250000000000003553, 2.750000000000000888, -10.00000000000000355 ) ) ;
#13316 = VERTEX_POINT ( 'NONE', #12024 ) ;
#13317 = COLOUR_RGB ( '',0.7921568627450980005, 0.8196078431372548767, 0.9333333333333333481 ) ;
#13318 = CARTESIAN_POINT ( 'NONE',  ( 4.577511697546072789, 3.000000000000000000, 12.75843939030335505 ) ) ;
#13319 = CIRCLE ( 'NONE', #7373, 1.500000000000001332 ) ;
#13320 = ADVANCED_FACE ( 'NONE', ( #2574 ), #9734, .T. ) ;
#13321 = ORIENTED_EDGE ( 'NONE', *, *, #10438, .F. ) ;
#13322 = EDGE_CURVE ( 'NONE', #1608, #1814, #315, .T. ) ;
#13323 = EDGE_CURVE ( 'NONE', #4042, #3324, #6483, .T. ) ;
#13324 = ORIENTED_EDGE ( 'NONE', *, *, #7064, .F. ) ;
#13325 = DIRECTION ( 'NONE',  ( -0.000000000000000000, -1.000000000000000000, -0.000000000000000000 ) ) ;
#13326 = VERTEX_POINT ( 'NONE', #3463 ) ;
#13327 = EDGE_CURVE ( 'NONE', #3458, #5440, #2967, .T. ) ;
#13328 = CYLINDRICAL_SURFACE ( 'NONE', #9771, 0.1000000000000000472 ) ;
#13329 = PRESENTATION_LAYER_ASSIGNMENT (  '', '', ( #2527 ) ) ;
#13330 = VECTOR ( 'NONE', #6589, 1000.000000000000000 ) ;
#13331 = FILL_AREA_STYLE ('',( #8212 ) ) ;
#13332 = DIRECTION ( 'NONE',  ( 0.000000000000000000, 1.000000000000000000, -0.000000000000000000 ) ) ;
#13333 = CARTESIAN_POINT ( 'NONE',  ( 10.34346111134700585, 0.000000000000000000, 8.760376775873716326 ) ) ;
#13334 = CARTESIAN_POINT ( 'NONE',  ( -3.833392836528145331, 9.000000000000000000, -5.555861711818853799 ) ) ;
#13335 = DIRECTION ( 'NONE',  ( 0.7772490812545796990, 0.000000000000000000, 0.6291930273683203900 ) ) ;
#13336 = DIRECTION ( 'NONE',  ( 0.000000000000000000, 0.000000000000000000, 1.000000000000000000 ) ) ;
#13337 = LINE ( 'NONE', #1693, #1787 ) ;
#13338 = CARTESIAN_POINT ( 'NONE',  ( 11.48836750521724070, 0.000000000000000000, -8.430890348300621895 ) ) ;
#13339 = CARTESIAN_POINT ( 'NONE',  ( -7.939678587550617728, 9.000000000000000000, 0.2057875656132798770 ) ) ;
#13340 = EDGE_CURVE ( 'NONE', #7698, #8964, #12915, .T. ) ;
#13341 = EDGE_LOOP ( 'NONE', ( #6552, #9474, #11647, #8399 ) ) ;
#13342 = PRESENTATION_LAYER_ASSIGNMENT (  '', '', ( #8259 ) ) ;
#13343 = ORIENTED_EDGE ( 'NONE', *, *, #3633, .F. ) ;
#13344 = ORIENTED_EDGE ( 'NONE', *, *, #8297, .T. ) ;
#13345 = EDGE_CURVE ( 'NONE', #4061, #3444, #9347, .T. ) ;
#13346 = VERTEX_POINT ( 'NONE', #10973 ) ;
#13347 = CARTESIAN_POINT ( 'NONE',  ( 4.690415759823430619, 2.900000000000000355, 4.500000000000000888 ) ) ;
#13348 = B_SPLINE_CURVE_WITH_KNOTS ( 'NONE', 3,
 ( #1509, #3638, #8938, #8790 ),
 .UNSPECIFIED., .F., .F.,
 ( 4, 4 ),
 ( 0.000000000000000000, 0.8724294488011762327 ),
 .UNSPECIFIED. ) ;
#13349 = DIRECTION ( 'NONE',  ( 0.000000000000000000, 0.000000000000000000, -1.000000000000000000 ) ) ;
#13350 = FACE_OUTER_BOUND ( 'NONE', #9237, .T. ) ;
#13351 = DIRECTION ( 'NONE',  ( 0.000000000000000000, 0.000000000000000000, -1.000000000000000000 ) ) ;
#13352 = DIRECTION ( 'NONE',  ( 0.000000000000000000, 0.000000000000000000, 1.000000000000000000 ) ) ;
#13353 = EDGE_CURVE ( 'NONE', #3503, #8945, #1873, .T. ) ;
#13354 = CARTESIAN_POINT ( 'NONE',  ( -13.04554897075799680, 0.000000000000000000, -5.733772933379471581 ) ) ;
#13355 = ORIENTED_EDGE ( 'NONE', *, *, #7731, .T. ) ;
#13356 = CARTESIAN_POINT ( 'NONE',  ( -6.549210654805285081, 0.000000000000000000, 1.634117437329677180 ) ) ;
#13357 = CARTESIAN_POINT ( 'NONE',  ( 0.000000000000000000, 3.000000000000000000, 0.000000000000000000 ) ) ;
#13358 = ORIENTED_EDGE ( 'NONE', *, *, #9849, .T. ) ;
#13359 = CARTESIAN_POINT ( 'NONE',  ( 0.000000000000000000, 3.000000000000000000, 0.000000000000000000 ) ) ;
#13360 = CARTESIAN_POINT ( 'NONE',  ( 36.17696780347059615, 35.33135765298362685, 55.45042399990210669 ) ) ;
#13361 = DIRECTION ( 'NONE',  ( 0.000000000000000000, 0.000000000000000000, -1.000000000000000000 ) ) ;
#13362 = CARTESIAN_POINT ( 'NONE',  ( 10.97318381393774089, 3.000000000000000000, -6.970598036433387712 ) ) ;
#13363 = CARTESIAN_POINT ( 'NONE',  ( 0.000000000000000000, 3.000000000000000000, 0.000000000000000000 ) ) ;
#13364 = CARTESIAN_POINT ( 'NONE',  ( 0.000000000000000000, 0.000000000000000000, 0.000000000000000000 ) ) ;
#13365 = ADVANCED_FACE ( 'NONE', ( #379 ), #8502, .F. ) ;
#13366 = DIRECTION ( 'NONE',  ( 0.000000000000000000, 0.000000000000000000, 1.000000000000000000 ) ) ;
#13367 = EDGE_CURVE ( 'NONE', #10549, #2066, #2930, .T. ) ;
#13368 = VERTEX_POINT ( 'NONE', #6635 ) ;
#13369 = FACE_OUTER_BOUND ( 'NONE', #4108, .T. ) ;
#13370 = ORIENTED_EDGE ( 'NONE', *, *, #9606, .T. ) ;
#13371 = ORIENTED_EDGE ( 'NONE', *, *, #8027, .T. ) ;
#13372 = CARTESIAN_POINT ( 'NONE',  ( 0.000000000000000000, 0.000000000000000000, 0.000000000000000000 ) ) ;
#13373 = ORIENTED_EDGE ( 'NONE', *, *, #12902, .F. ) ;
#13374 = ORIENTED_EDGE ( 'NONE', *, *, #5677, .F. ) ;
#13375 = CARTESIAN_POINT ( 'NONE',  ( 8.883544964651964193, 0.000000000000000000, -12.08646469655236544 ) ) ;
#13376 = FILL_AREA_STYLE ('',( #13310 ) ) ;
#13377 = CARTESIAN_POINT ( 'NONE',  ( -12.68816982652970893, 3.000000000000000000, 2.830255545554337004 ) ) ;
#13378 = FACE_OUTER_BOUND ( 'NONE', #8332, .T. ) ;
#13379 = LINE ( 'NONE', #7183, #972 ) ;
#13380 = CARTESIAN_POINT ( 'NONE',  ( 26.30958424017656938, 2.900000000000000355, -1.500000000000000000 ) ) ;
#13381 = CARTESIAN_POINT ( 'NONE',  ( 0.7944557581062194895, 0.000000000000000000, -6.703084368289861317 ) ) ;
#13382 = ORIENTED_EDGE ( 'NONE', *, *, #6763, .F. ) ;
#13383 = CARTESIAN_POINT ( 'NONE',  ( 0.000000000000000000, 3.000000000000000000, -1.399999999999999911 ) ) ;
#13384 = ORIENTED_EDGE ( 'NONE', *, *, #11392, .F. ) ;
#13385 = EDGE_LOOP ( 'NONE', ( #9723, #7492, #2550, #3157 ) ) ;
#13386 = LINE ( 'NONE', #3933, #8186 ) ;
#13387 = VERTEX_POINT ( 'NONE', #11872 ) ;
#13388 =( REPRESENTATION_RELATIONSHIP ('NONE','NONE', #3798, #7939 ) REPRESENTATION_RELATIONSHIP_WITH_TRANSFORMATION ( #11455 )SHAPE_REPRESENTATION_RELATIONSHIP( ) );
#13389 = B_SPLINE_CURVE_WITH_KNOTS ( 'NONE', 3,
 ( #6141, #2147, #984, #10490 ),
 .UNSPECIFIED., .F., .F.,
 ( 4, 4 ),
 ( 0.1276832474596253097, 1.000000000000000000 ),
 .UNSPECIFIED. ) ;
#13390 = CARTESIAN_POINT ( 'NONE',  ( 8.914835885878279242, 0.000000000000000000, 11.11702303352191734 ) ) ;
#13391 = CARTESIAN_POINT ( 'NONE',  ( 11.90284147956858085, 0.000000000000000000, -9.133371500908429752 ) ) ;
#13392 = DIRECTION ( 'NONE',  ( -2.312964634635735561E-15, -1.000000000000000000, 0.000000000000000000 ) ) ;
#13393 = EDGE_CURVE ( 'NONE', #9896, #11420, #10843, .T. ) ;
#13394 = PLANE ( 'NONE',  #11222 ) ;
#13395 = FACE_OUTER_BOUND ( 'NONE', #8078, .T. ) ;
#13396 = CARTESIAN_POINT ( 'NONE',  ( 5.741477348071313713, 0.000000000000000000, -13.86115248177180703 ) ) ;
#13397 = CARTESIAN_POINT ( 'NONE',  ( -4.174571361198896824, 0.000000000000000000, 6.065330394303907191 ) ) ;
#13398 = LINE ( 'NONE', #11336, #2713 ) ;
#13399 = DIRECTION ( 'NONE',  ( -0.000000000000000000, -1.000000000000000000, -0.000000000000000000 ) ) ;
#13400 = ORIENTED_EDGE ( 'NONE', *, *, #8352, .T. ) ;
#13401 = VERTEX_POINT ( 'NONE', #10769 ) ;
#13402 = ORIENTED_EDGE ( 'NONE', *, *, #448, .T. ) ;
#13403 = VERTEX_POINT ( 'NONE', #11041 ) ;
#13404 = CARTESIAN_POINT ( 'NONE',  ( -8.352599575481690408, 0.000000000000000000, 28.00000000000000000 ) ) ;
#13405 = CARTESIAN_POINT ( 'NONE',  ( -9.379342464487789854, 0.000000000000000000, -10.98198414889931307 ) ) ;
#13406 = EDGE_CURVE ( 'NONE', #11587, #13346, #2518, .T. ) ;
#13407 = CARTESIAN_POINT ( 'NONE',  ( 0.000000000000000000, 13.00000000000000178, 0.000000000000000000 ) ) ;
#13408 = FACE_BOUND ( 'NONE', #9458, .T. ) ;
#13409 = CARTESIAN_POINT ( 'NONE',  ( -2.631756770590896632, 0.000000000000000000, -14.20034848914872505 ) ) ;
#13410 = EDGE_CURVE ( 'NONE', #284, #7698, #5074, .T. ) ;
#13411 = EDGE_CURVE ( 'NONE', #5856, #9614, #8966, .T. ) ;
#13412 = AXIS2_PLACEMENT_3D ( 'NONE', #3904, #3973, #12407 ) ;
#13413 = DIRECTION ( 'NONE',  ( 0.000000000000000000, 1.000000000000000000, 0.000000000000000000 ) ) ;
#13414 = FACE_OUTER_BOUND ( 'NONE', #3591, .T. ) ;
#13415 = VERTEX_POINT ( 'NONE', #794 ) ;
#13416 = MANIFOLD_SOLID_BREP ( 'Boss-Extrude2', #5104 ) ;
#13417 = DIRECTION ( 'NONE',  ( 0.000000000000000000, 0.000000000000000000, -1.000000000000000000 ) ) ;
#13418 = CARTESIAN_POINT ( 'NONE',  ( -3.893011711613112880, 0.000000000000000000, -12.40340517008282717 ) ) ;
#13419 = EDGE_LOOP ( 'NONE', ( #8303, #5052 ) ) ;
#13420 = EDGE_CURVE ( 'NONE', #8421, #11907, #4905, .T. ) ;
#13421 = CIRCLE ( 'NONE', #3512, 1.500000000000000222 ) ;
#13422 = CARTESIAN_POINT ( 'NONE',  ( 0.000000000000000000, 3.000000000000000000, 0.000000000000000000 ) ) ;
#13423 = CARTESIAN_POINT ( 'NONE',  ( -12.55526518755974585, 3.000000000000000000, -2.546103534247746047 ) ) ;
#13424 = DIRECTION ( 'NONE',  ( -1.000000000000000000, -0.000000000000000000, -0.000000000000000000 ) ) ;
#13425 = DIRECTION ( 'NONE',  ( 0.000000000000000000, 0.000000000000000000, -1.000000000000000000 ) ) ;
#13426 = DIRECTION ( 'NONE',  ( 0.000000000000000000, 1.000000000000000000, 0.000000000000000000 ) ) ;
#13427 = DIRECTION ( 'NONE',  ( 0.000000000000000000, 0.000000000000000000, -1.000000000000000000 ) ) ;
#13428 = VERTEX_POINT ( 'NONE', #4984 ) ;
#13429 = CARTESIAN_POINT ( 'NONE',  ( -9.600126836553261711, 3.000000000000000000, -8.482622935103767858 ) ) ;
#13430 = AXIS2_PLACEMENT_3D ( 'NONE', #2267, #4402, #2343 ) ;
#13431 = ORIENTED_EDGE ( 'NONE', *, *, #9016, .F. ) ;
#13432 = MECHANICAL_DESIGN_GEOMETRIC_PRESENTATION_REPRESENTATION (  '', ( #5288 ), #10345 ) ;
#13433 = UNCERTAINTY_MEASURE_WITH_UNIT (LENGTH_MEASURE( 1.000000000000000082E-05 ), #5357, 'distance_accuracy_value', 'NONE');
#13434 = ORIENTED_EDGE ( 'NONE', *, *, #6355, .T. ) ;
#13435 = CARTESIAN_POINT ( 'NONE',  ( -12.40347894490204972, 0.000000000000000000, 3.892776652129660064 ) ) ;
#13436 = EDGE_LOOP ( 'NONE', ( #12755, #2629, #6827, #6194 ) ) ;
#13437 = ADVANCED_FACE ( 'NONE', ( #9177 ), #3228, .F. ) ;
#13438 = EDGE_CURVE ( 'NONE', #8770, #3702, #11565, .T. ) ;
#13439 = CARTESIAN_POINT ( 'NONE',  ( -11.14709020439930676, 0.000000000000000000, -7.712570079660886257 ) ) ;
#13440 =( NAMED_UNIT ( * ) SI_UNIT ( $, .STERADIAN. ) SOLID_ANGLE_UNIT ( ) );
#13441 = VECTOR ( 'NONE', #6418, 1000.000000000000000 ) ;
#13442 = DIRECTION ( 'NONE',  ( -3.357529308342206122E-15, 0.000000000000000000, 1.000000000000000000 ) ) ;
#13443 = DIRECTION ( 'NONE',  ( -1.000000000000000000, 3.469446951953610639E-15, 2.602085213965210149E-16 ) ) ;
#13444 = CIRCLE ( 'NONE', #1561, 3.000000000000000888 ) ;
#13445 = CARTESIAN_POINT ( 'NONE',  ( -9.299128225235689271, 0.000000000000000000, -10.25006213149501555 ) ) ;
#13446 = EDGE_CURVE ( 'NONE', #7415, #1162, #2777, .T. ) ;
#13447 = DIRECTION ( 'NONE',  ( 0.000000000000000000, 0.000000000000000000, -1.000000000000000000 ) ) ;
#13448 = DIRECTION ( 'NONE',  ( 3.469446951953610639E-15, 1.000000000000000000, 2.891205793294675861E-16 ) ) ;
#13449 = B_SPLINE_CURVE_WITH_KNOTS ( 'NONE', 3,
 ( #5371, #9578, #7507, #9640 ),
 .UNSPECIFIED., .F., .F.,
 ( 4, 4 ),
 ( 0.000000000000000000, 0.8452273900860258760 ),
 .UNSPECIFIED. ) ;
#13450 = ORIENTED_EDGE ( 'NONE', *, *, #4930, .T. ) ;
#13451 = CARTESIAN_POINT ( 'NONE',  ( -2.411622991978543684, 9.000000000000000000, -6.304488444319686913 ) ) ;
#13452 = ADVANCED_BREP_SHAPE_REPRESENTATION ( '', ( #13099, #10007 ), #12883 ) ;
#13453 = VERTEX_POINT ( 'NONE', #7128 ) ;
#13454 = ORIENTED_EDGE ( 'NONE', *, *, #7014, .F. ) ;
#13455 = LINE ( 'NONE', #1421, #12393 ) ;
#13456 = VECTOR ( 'NONE', #591, 1000.000000000000000 ) ;
#13457 = VECTOR ( 'NONE', #9120, 1000.000000000000000 ) ;
#13458 = ORIENTED_EDGE ( 'NONE', *, *, #12506, .F. ) ;
#13459 = CARTESIAN_POINT ( 'NONE',  ( 26.30958424017656938, 0.000000000000000000, 1.399999999999999911 ) ) ;
#13460 = DIRECTION ( 'NONE',  ( 0.000000000000000000, 0.000000000000000000, 1.000000000000000000 ) ) ;
#13461 = DIRECTION ( 'NONE',  ( 0.000000000000000000, 1.000000000000000000, -0.000000000000000000 ) ) ;
#13462 = DIRECTION ( 'NONE',  ( 0.000000000000000000, 1.000000000000000000, -0.000000000000000000 ) ) ;
#13463 = CARTESIAN_POINT ( 'NONE',  ( 0.000000000000000000, 2.900000000000000355, -1.500000000000000000 ) ) ;
#13464 = VECTOR ( 'NONE', #2292, 1000.000000000000000 ) ;
#13465 = CARTESIAN_POINT ( 'NONE',  ( -7.723663868796776910, 0.000000000000000000, -11.13895890373326303 ) ) ;
#13466 = CYLINDRICAL_SURFACE ( 'NONE', #5095, 1.000000000000001776 ) ;
#13467 = ORIENTED_EDGE ( 'NONE', *, *, #8537, .T. ) ;
#13468 = DIRECTION ( 'NONE',  ( 0.000000000000000000, 0.000000000000000000, -1.000000000000000000 ) ) ;
#13469 = VERTEX_POINT ( 'NONE', #4086 ) ;
#13470 = ORIENTED_EDGE ( 'NONE', *, *, #8564, .F. ) ;
#13471 = EDGE_CURVE ( 'NONE', #10501, #6263, #9351, .T. ) ;
#13472 = EDGE_LOOP ( 'NONE', ( #5483, #8693, #2696, #1364 ) ) ;
#13473 = AXIS2_PLACEMENT_3D ( 'NONE', #3261, #11294, #4314 ) ;
#13474 = VERTEX_POINT ( 'NONE', #12230 ) ;
#13475 = CARTESIAN_POINT ( 'NONE',  ( -3.893011711613112880, 3.000000000000000000, -12.40340517008282717 ) ) ;
#13476 = DIRECTION ( 'NONE',  ( -0.8149588969772670888, 0.000000000000000000, 0.5795187626277481518 ) ) ;
#13477 = LINE ( 'NONE', #9408, #9740 ) ;
#13478 = DIRECTION ( 'NONE',  ( 0.000000000000000000, -1.000000000000000000, 0.000000000000000000 ) ) ;
#13479 = CYLINDRICAL_SURFACE ( 'NONE', #3980, 1.000000000000000000 ) ;
#13480 = CIRCLE ( 'NONE', #8404, 14.24999999999999822 ) ;
#13481 = AXIS2_PLACEMENT_3D ( 'NONE', #9591, #6623, #3510 ) ;
#13482 = CARTESIAN_POINT ( 'NONE',  ( 8.430890348300586368, 3.000000000000000000, -11.48836750521726913 ) ) ;
#13483 = CARTESIAN_POINT ( 'NONE',  ( -14.08504230442587790, 0.000000000000000000, -2.161962830978695571 ) ) ;
#13484 = ORIENTED_EDGE ( 'NONE', *, *, #6113, .T. ) ;
#13485 = DIRECTION ( 'NONE',  ( -0.000000000000000000, -1.000000000000000000, -0.000000000000000000 ) ) ;
#13486 = CYLINDRICAL_SURFACE ( 'NONE', #1611, 2.500000000000000000 ) ;
#13487 = ORIENTED_EDGE ( 'NONE', *, *, #8172, .T. ) ;
#13488 = CIRCLE ( 'NONE', #9738, 1.600000000000000311 ) ;
#13489 = ADVANCED_FACE ( 'NONE', ( #6089 ), #851, .T. ) ;
#13490 = VECTOR ( 'NONE', #3753, 1000.000000000000000 ) ;
#13491 = EDGE_CURVE ( 'NONE', #8876, #3254, #9516, .T. ) ;
#13492 = VECTOR ( 'NONE', #5915, 1000.000000000000000 ) ;
#13493 = CARTESIAN_POINT ( 'NONE',  ( 0.000000000000000000, 9.000000000000000000, 0.000000000000000000 ) ) ;
#13494 = PRODUCT_CONTEXT ( 'NONE', #713, 'mechanical' ) ;
#13495 = CARTESIAN_POINT ( 'NONE',  ( 0.5400000000008001733, 3.000000000000000000, 12.07793442604883616 ) ) ;
#13496 = CARTESIAN_POINT ( 'NONE',  ( 4.564691384634508964, 0.000000000000000000, -12.76342233970727413 ) ) ;
#13497 = CARTESIAN_POINT ( 'NONE',  ( 5.571433138827823761, 0.000000000000000000, 10.72973591378220704 ) ) ;
#13498 = DIRECTION ( 'NONE',  ( -0.000000000000000000, -1.000000000000000000, 0.000000000000000000 ) ) ;
#13499 = B_SPLINE_CURVE_WITH_KNOTS ( 'NONE', 3,
 ( #6524, #8573, #12796, #7559 ),
 .UNSPECIFIED., .F., .F.,
 ( 4, 4 ),
 ( 0.000000000000000000, 0.8452273900860258760 ),
 .UNSPECIFIED. ) ;
#13500 = VECTOR ( 'NONE', #11543, 1000.000000000000000 ) ;
#13501 = DIRECTION ( 'NONE',  ( 0.000000000000000000, 0.000000000000000000, 1.000000000000000000 ) ) ;
#13502 = AXIS2_PLACEMENT_3D ( 'NONE', #8358, #7276, #8495 ) ;
#13503 = VECTOR ( 'NONE', #10995, 1000.000000000000000 ) ;
#13504 = EDGE_CURVE ( 'NONE', #9031, #1237, #5114, .T. ) ;
#13505 = ORIENTED_EDGE ( 'NONE', *, *, #4761, .T. ) ;
#13506 = EDGE_LOOP ( 'NONE', ( #11279, #13076, #10531, #5579 ) ) ;
#13507 = DIRECTION ( 'NONE',  ( 0.000000000000000000, 0.000000000000000000, 1.000000000000000000 ) ) ;
#13508 = ORIENTED_EDGE ( 'NONE', *, *, #2402, .T. ) ;
#13509 = ADVANCED_FACE ( 'NONE', ( #9590 ), #9651, .F. ) ;
#13510 = CARTESIAN_POINT ( 'NONE',  ( 30.73000000000000043, 3.000000000000000000, -3.999999999999999112 ) ) ;
#13511 = VECTOR ( 'NONE', #314, 1000.000000000000000 ) ;
#13512 =( NAMED_UNIT ( * ) SI_UNIT ( $, .STERADIAN. ) SOLID_ANGLE_UNIT ( ) );
#13513 = AXIS2_PLACEMENT_3D ( 'NONE', #572, #8953, #5716 ) ;
#13514 = CARTESIAN_POINT ( 'NONE',  ( -0.5501230721523990841, 0.000000000000000000, -12.98835496148299384 ) ) ;
#13515 = CARTESIAN_POINT ( 'NONE',  ( -3.533475733155563070, 0.000000000000000000, 7.730753471893976325 ) ) ;
#13516 = DIRECTION ( 'NONE',  ( 0.000000000000000000, 0.000000000000000000, 1.000000000000000000 ) ) ;
#13517 = CARTESIAN_POINT ( 'NONE',  ( 9.375397774054407662, 3.000000000000000000, -11.70905276178460497 ) ) ;
#13518 = CARTESIAN_POINT ( 'NONE',  ( -12.40340517008309185, 0.000000000000000000, -3.893011711613028947 ) ) ;
#13519 = ORIENTED_EDGE ( 'NONE', *, *, #11210, .T. ) ;
#13520 = CARTESIAN_POINT ( 'NONE',  ( -14.82803603298498629, 0.000000000000000000, 2.264806262023049577 ) ) ;
#13521 = EDGE_CURVE ( 'NONE', #12863, #6179, #782, .T. ) ;
#13522 = ORIENTED_EDGE ( 'NONE', *, *, #460, .F. ) ;
#13523 = ADVANCED_FACE ( 'NONE', ( #1052 ), #10494, .F. ) ;
#13524 = VECTOR ( 'NONE', #1489, 1000.000000000000227 ) ;
#13525 = ORIENTED_EDGE ( 'NONE', *, *, #12490, .T. ) ;
#13526 = AXIS2_PLACEMENT_3D ( 'NONE', #11364, #5982, #6186 ) ;
#13527 = CARTESIAN_POINT ( 'NONE',  ( -3.893011711613112880, 0.000000000000000000, -12.40340517008282717 ) ) ;
#13528 = VERTEX_POINT ( 'NONE', #3308 ) ;
#13529 = CARTESIAN_POINT ( 'NONE',  ( 1.650143266773734796, 3.000000000000000000, -14.90895795148410841 ) ) ;
#13530 = CARTESIAN_POINT ( 'NONE',  ( 8.922136023539611216, 0.000000000000000000, -8.158651161643899030 ) ) ;
#13531 = CARTESIAN_POINT ( 'NONE',  ( 7.723663868796767140, 3.000000000000000000, 11.13895890373327191 ) ) ;
#13532 = CARTESIAN_POINT ( 'NONE',  ( -2.604531154829235362, 3.000000000000000000, -11.80612203322752585 ) ) ;
#13533 = CARTESIAN_POINT ( 'NONE',  ( 31.00000000000000000, 3.000000000000000000, -1.073670993220974656E-09 ) ) ;
#13534 = CARTESIAN_POINT ( 'NONE',  ( 8.883544964651964193, 3.000000000000000000, -12.08646469655236544 ) ) ;
#13535 = AXIS2_PLACEMENT_3D ( 'NONE', #6898, #6007, #10211 ) ;
#13536 = CARTESIAN_POINT ( 'NONE',  ( 2.458659560121116527, 0.000000000000000000, -8.136645080586040635 ) ) ;
#13537 = CARTESIAN_POINT ( 'NONE',  ( -9.573149624528719315, 0.000000000000000000, -8.795158114916407754 ) ) ;
#13538 = CARTESIAN_POINT ( 'NONE',  ( -7.723663868796776910, 0.000000000000000000, -11.13895890373326303 ) ) ;
#13539 = AXIS2_PLACEMENT_3D ( 'NONE', #7317, #9715, #3106 ) ;
#13540 = ORIENTED_EDGE ( 'NONE', *, *, #5835, .F. ) ;
#13541 = DIRECTION ( 'NONE',  ( -0.000000000000000000, -1.000000000000000000, -0.000000000000000000 ) ) ;
#13542 = ORIENTED_EDGE ( 'NONE', *, *, #4899, .F. ) ;
#13543 = ADVANCED_FACE ( 'NONE', ( #5446 ), #5192, .F. ) ;
#13544 = ORIENTED_EDGE ( 'NONE', *, *, #11908, .T. ) ;
#13545 = ORIENTED_EDGE ( 'NONE', *, *, #448, .F. ) ;
#13546 = ORIENTED_EDGE ( 'NONE', *, *, #9034, .F. ) ;
#13547 = CARTESIAN_POINT ( 'NONE',  ( 19.44487669093179605, 3.000000000000000000, -16.66326752702930847 ) ) ;
#13548 = DIRECTION ( 'NONE',  ( -0.000000000000000000, -1.000000000000000000, -0.000000000000000000 ) ) ;
#13549 = DIRECTION ( 'NONE',  ( 0.000000000000000000, 0.000000000000000000, 1.000000000000000000 ) ) ;
#13550 = FACE_OUTER_BOUND ( 'NONE', #4907, .T. ) ;
#13551 = EDGE_CURVE ( 'NONE', #4042, #746, #9520, .T. ) ;
#13552 = CARTESIAN_POINT ( 'NONE',  ( -14.16466328168010769, 0.000000000000000000, -1.557181465540670384 ) ) ;
#13553 = CARTESIAN_POINT ( 'NONE',  ( -1.557181465540677712, 3.000000000000000000, 14.16466328168010769 ) ) ;
#13554 = ORIENTED_EDGE ( 'NONE', *, *, #5506, .F. ) ;
#13555 = DIRECTION ( 'NONE',  ( 0.000000000000000000, -1.000000000000000000, 0.000000000000000000 ) ) ;
#13556 = DIRECTION ( 'NONE',  ( -0.000000000000000000, -1.000000000000000000, -0.000000000000000000 ) ) ;
#13557 = EDGE_LOOP ( 'NONE', ( #446, #7390, #3660, #12913 ) ) ;
#13558 = B_SPLINE_SURFACE_WITH_KNOTS ( 'NONE', 3, 1, ( 
 ( #2493, #421 ),
 ( #1466, #5653 ),
 ( #4132, #1940 ),
 ( #5928, #2972 ) ),
 .UNSPECIFIED., .F., .F., .F.,
 ( 4, 4 ),
 ( 2, 2 ),
 ( 0.000000000000000000, 0.8724294488011784532 ),
 ( 0.000000000000000000, 1.000000000000000000 ),
 .UNSPECIFIED. ) ;
#13559 = CYLINDRICAL_SURFACE ( 'NONE', #3152, 12.08999999999737440 ) ;
#13560 = DIRECTION ( 'NONE',  ( -0.000000000000000000, -1.000000000000000000, -0.000000000000000000 ) ) ;
#13561 = APPLICATION_PROTOCOL_DEFINITION ( 'draft international standard', 'automotive_design', 1998, #2816 ) ;
#13562 = DIRECTION ( 'NONE',  ( 0.000000000000000000, 0.000000000000000000, 1.000000000000000000 ) ) ;
#13563 = CARTESIAN_POINT ( 'NONE',  ( 22.00000000000000000, 3.000000000000000000, 0.000000000000000000 ) ) ;
#13564 = EDGE_CURVE ( 'NONE', #4061, #2104, #7520, .T. ) ;
#13565 = CARTESIAN_POINT ( 'NONE',  ( -3.833392836528144443, 9.000000000000000000, -5.555861711818853799 ) ) ;
#13566 = CARTESIAN_POINT ( 'NONE',  ( 0.000000000000000000, 3.000000000000000000, 0.000000000000000000 ) ) ;
#13567 = CARTESIAN_POINT ( 'NONE',  ( 5.517918333394296049, 9.000000000000000000, 4.875228826198821253 ) ) ;
#13568 = EDGE_LOOP ( 'NONE', ( #10764, #12530, #1460, #13174 ) ) ;
#13569 = ORIENTED_EDGE ( 'NONE', *, *, #4365, .F. ) ;
#13570 = ORIENTED_EDGE ( 'NONE', *, *, #1269, .F. ) ;
#13571 = CARTESIAN_POINT ( 'NONE',  ( 52.34174591811297717, 0.000000000000000000, -12.24483450274845531 ) ) ;
#13572 = EDGE_LOOP ( 'NONE', ( #10471, #8947 ) ) ;
#13573 = CARTESIAN_POINT ( 'NONE',  ( 9.065480927540312095, 3.000000000000000000, -9.324856600128422102 ) ) ;
#13574 = CYLINDRICAL_SURFACE ( 'NONE', #8406, 12.08999999999737440 ) ;
#13575 = ADVANCED_FACE ( 'NONE', ( #6284 ), #1147, .F. ) ;
#13576 = LINE ( 'NONE', #6199, #9018 ) ;
#13577 = CARTESIAN_POINT ( 'NONE',  ( 4.690415759823430619, 2.900000000000000355, 1.500000000000000000 ) ) ;
#13578 = EDGE_CURVE ( 'NONE', #1090, #8924, #3045, .T. ) ;
#13579 = CARTESIAN_POINT ( 'NONE',  ( -5.065227977808753224, 9.000000000000000000, -4.461610195077944319 ) ) ;
#13580 = CARTESIAN_POINT ( 'NONE',  ( -13.04554897075799680, 0.000000000000000000, -5.733772933379471581 ) ) ;
#13581 = EDGE_LOOP ( 'NONE', ( #6388, #2396 ) ) ;
#13582 = EDGE_CURVE ( 'NONE', #11262, #6390, #5249, .T. ) ;
#13583 = CARTESIAN_POINT ( 'NONE',  ( 13.50000000000000355, 3.000000000000000000, -7.050000000000000711 ) ) ;
#13584 = ADVANCED_FACE ( 'NONE', ( #7255 ), #10424, .F. ) ;
#13585 = ORIENTED_EDGE ( 'NONE', *, *, #7363, .F. ) ;
#13586 = ORIENTED_EDGE ( 'NONE', *, *, #4365, .T. ) ;
#13587 = CYLINDRICAL_SURFACE ( 'NONE', #10174, 1.500000000000003997 ) ;
#13588 = ORIENTED_EDGE ( 'NONE', *, *, #10021, .T. ) ;
#13589 = AXIS2_PLACEMENT_3D ( 'NONE', #7850, #4554, #12138 ) ;
#13590 = LINE ( 'NONE', #6018, #2520 ) ;
#13591 = CARTESIAN_POINT ( 'NONE',  ( 2.604399508763944660, 3.000000000000000000, -11.80615107470197600 ) ) ;
#13592 = CARTESIAN_POINT ( 'NONE',  ( 9.250000000000001776, 1.999999999999998224, -10.00000000000000355 ) ) ;
#13593 = CARTESIAN_POINT ( 'NONE',  ( 9.600126836553261711, 0.000000000000000000, 8.482622935103766082 ) ) ;
#13594 = CARTESIAN_POINT ( 'NONE',  ( -5.571313494980132397, 3.000000000000000000, 10.72979803820132005 ) ) ;
#13595 = FACE_OUTER_BOUND ( 'NONE', #10965, .T. ) ;
#13596 = CARTESIAN_POINT ( 'NONE',  ( -2.830255545554292151, 0.000000000000000000, -12.68816982652971959 ) ) ;
#13597 = NEXT_ASSEMBLY_USAGE_OCCURRENCE ( 'NAUO1', ' ', ' ', #10179, #3028, $ ) ;
#13598 = NEXT_ASSEMBLY_USAGE_OCCURRENCE ( 'NAUO2', ' ', ' ', #10179, #3028, $ ) ;
#13599 = NEXT_ASSEMBLY_USAGE_OCCURRENCE ( 'NAUO3', ' ', ' ', #10179, #10940, $ ) ;
#13600 = NEXT_ASSEMBLY_USAGE_OCCURRENCE ( 'NAUO4', ' ', ' ', #10179, #5460, $ ) ;
#13601 = NEXT_ASSEMBLY_USAGE_OCCURRENCE ( 'NAUO5', ' ', ' ', #10179, #5460, $ ) ;
#13602 = NEXT_ASSEMBLY_USAGE_OCCURRENCE ( 'NAUO6', ' ', ' ', #10179, #1605, $ ) ;
#13603 = NEXT_ASSEMBLY_USAGE_OCCURRENCE ( 'NAUO7', ' ', ' ', #10179, #1605, $ ) ;
#13604 = NEXT_ASSEMBLY_USAGE_OCCURRENCE ( 'NAUO8', ' ', ' ', #10179, #1605, $ ) ;
#13605 = NEXT_ASSEMBLY_USAGE_OCCURRENCE ( 'NAUO9', ' ', ' ', #10179, #1605, $ ) ;
#13606 = NEXT_ASSEMBLY_USAGE_OCCURRENCE ( 'NAUO10', ' ', ' ', #10179, #5706, $ ) ;
#13607 = NEXT_ASSEMBLY_USAGE_OCCURRENCE ( 'NAUO11', ' ', ' ', #10179, #10603, $ ) ;
#13608 = NEXT_ASSEMBLY_USAGE_OCCURRENCE ( 'NAUO12', ' ', ' ', #10179, #10603, $ ) ;
#13609 = NEXT_ASSEMBLY_USAGE_OCCURRENCE ( 'NAUO13', ' ', ' ', #10179, #10603, $ ) ;
#13610 = NEXT_ASSEMBLY_USAGE_OCCURRENCE ( 'NAUO14', ' ', ' ', #10179, #4289, $ ) ;
#13611 = NEXT_ASSEMBLY_USAGE_OCCURRENCE ( 'NAUO15', ' ', ' ', #10179, #10603, $ ) ;
#13612 = NEXT_ASSEMBLY_USAGE_OCCURRENCE ( 'NAUO16', ' ', ' ', #10179, #10603, $ ) ;
#13613 = NEXT_ASSEMBLY_USAGE_OCCURRENCE ( 'NAUO17', ' ', ' ', #10179, #11618, $ ) ;
#13614 = NEXT_ASSEMBLY_USAGE_OCCURRENCE ( 'NAUO18', ' ', ' ', #10179, #4289, $ ) ;
#13615 = NEXT_ASSEMBLY_USAGE_OCCURRENCE ( 'NAUO19', ' ', ' ', #10179, #4289, $ ) ;
#13616 = NEXT_ASSEMBLY_USAGE_OCCURRENCE ( 'NAUO20', ' ', ' ', #10179, #4289, $ ) ;
#13617 = NEXT_ASSEMBLY_USAGE_OCCURRENCE ( 'NAUO21', ' ', ' ', #10179, #4289, $ ) ;
#13618 = NEXT_ASSEMBLY_USAGE_OCCURRENCE ( 'NAUO22', ' ', ' ', #10179, #4289, $ ) ;
#13619 = NEXT_ASSEMBLY_USAGE_OCCURRENCE ( 'NAUO23', ' ', ' ', #10179, #4289, $ ) ;
#13620 = NEXT_ASSEMBLY_USAGE_OCCURRENCE ( 'NAUO24', ' ', ' ', #10179, #4289, $ ) ;
#13621 = NEXT_ASSEMBLY_USAGE_OCCURRENCE ( 'NAUO25', ' ', ' ', #10179, #10603, $ ) ;
#13622=COLOUR_RGB('Dark Blue',0.08,0.2,0.34);
#13623=FILL_AREA_STYLE_COLOUR('',#13622);
#13624=FILL_AREA_STYLE('',(#13623));
#13625=SURFACE_STYLE_FILL_AREA(#13624);
#13626=SURFACE_SIDE_STYLE('',(#13625));
#13627=SURFACE_STYLE_USAGE(.BOTH.,#13626);
#13628=PRESENTATION_STYLE_ASSIGNMENT((#13627));
#13629=COLOUR_RGB('Light Blue',0.38,0.62,0.78);
#13630=FILL_AREA_STYLE_COLOUR('',#13629);
#13631=FILL_AREA_STYLE('',(#13630));
#13632=SURFACE_STYLE_FILL_AREA(#13631);
#13633=SURFACE_SIDE_STYLE('',(#13632));
#13634=SURFACE_STYLE_USAGE(.BOTH.,#13633);
#13635=PRESENTATION_STYLE_ASSIGNMENT((#13634));
#13636=COLOUR_RGB('Sky Blue',0.24,0.69,0.87);
#13637=FILL_AREA_STYLE_COLOUR('',#13636);
#13638=FILL_AREA_STYLE('',(#13637));
#13639=SURFACE_STYLE_FILL_AREA(#13638);
#13640=SURFACE_SIDE_STYLE('',(#13639));
#13641=SURFACE_STYLE_USAGE(.BOTH.,#13640);
#13642=PRESENTATION_STYLE_ASSIGNMENT((#13641));
#13643=COLOUR_RGB('Grey',0.48,0.52,0.57);
#13644=FILL_AREA_STYLE_COLOUR('',#13643);
#13645=FILL_AREA_STYLE('',(#13644));
#13646=SURFACE_STYLE_FILL_AREA(#13645);
#13647=SURFACE_SIDE_STYLE('',(#13646));
#13648=SURFACE_STYLE_USAGE(.BOTH.,#13647);
#13649=PRESENTATION_STYLE_ASSIGNMENT((#13648));
#13650=COLOUR_RGB('Black',0.12,0.14,0.17);
#13651=FILL_AREA_STYLE_COLOUR('',#13650);
#13652=FILL_AREA_STYLE('',(#13651));
#13653=SURFACE_STYLE_FILL_AREA(#13652);
#13654=SURFACE_SIDE_STYLE('',(#13653));
#13655=SURFACE_STYLE_USAGE(.BOTH.,#13654);
#13656=PRESENTATION_STYLE_ASSIGNMENT((#13655));
#13657=COLOUR_RGB('Off White',0.89,0.88,0.83);
#13658=FILL_AREA_STYLE_COLOUR('',#13657);
#13659=FILL_AREA_STYLE('',(#13658));
#13660=SURFACE_STYLE_FILL_AREA(#13659);
#13661=SURFACE_SIDE_STYLE('',(#13660));
#13662=SURFACE_STYLE_USAGE(.BOTH.,#13661);
#13663=PRESENTATION_STYLE_ASSIGNMENT((#13662));
ENDSEC;
END-ISO-10303-21;
